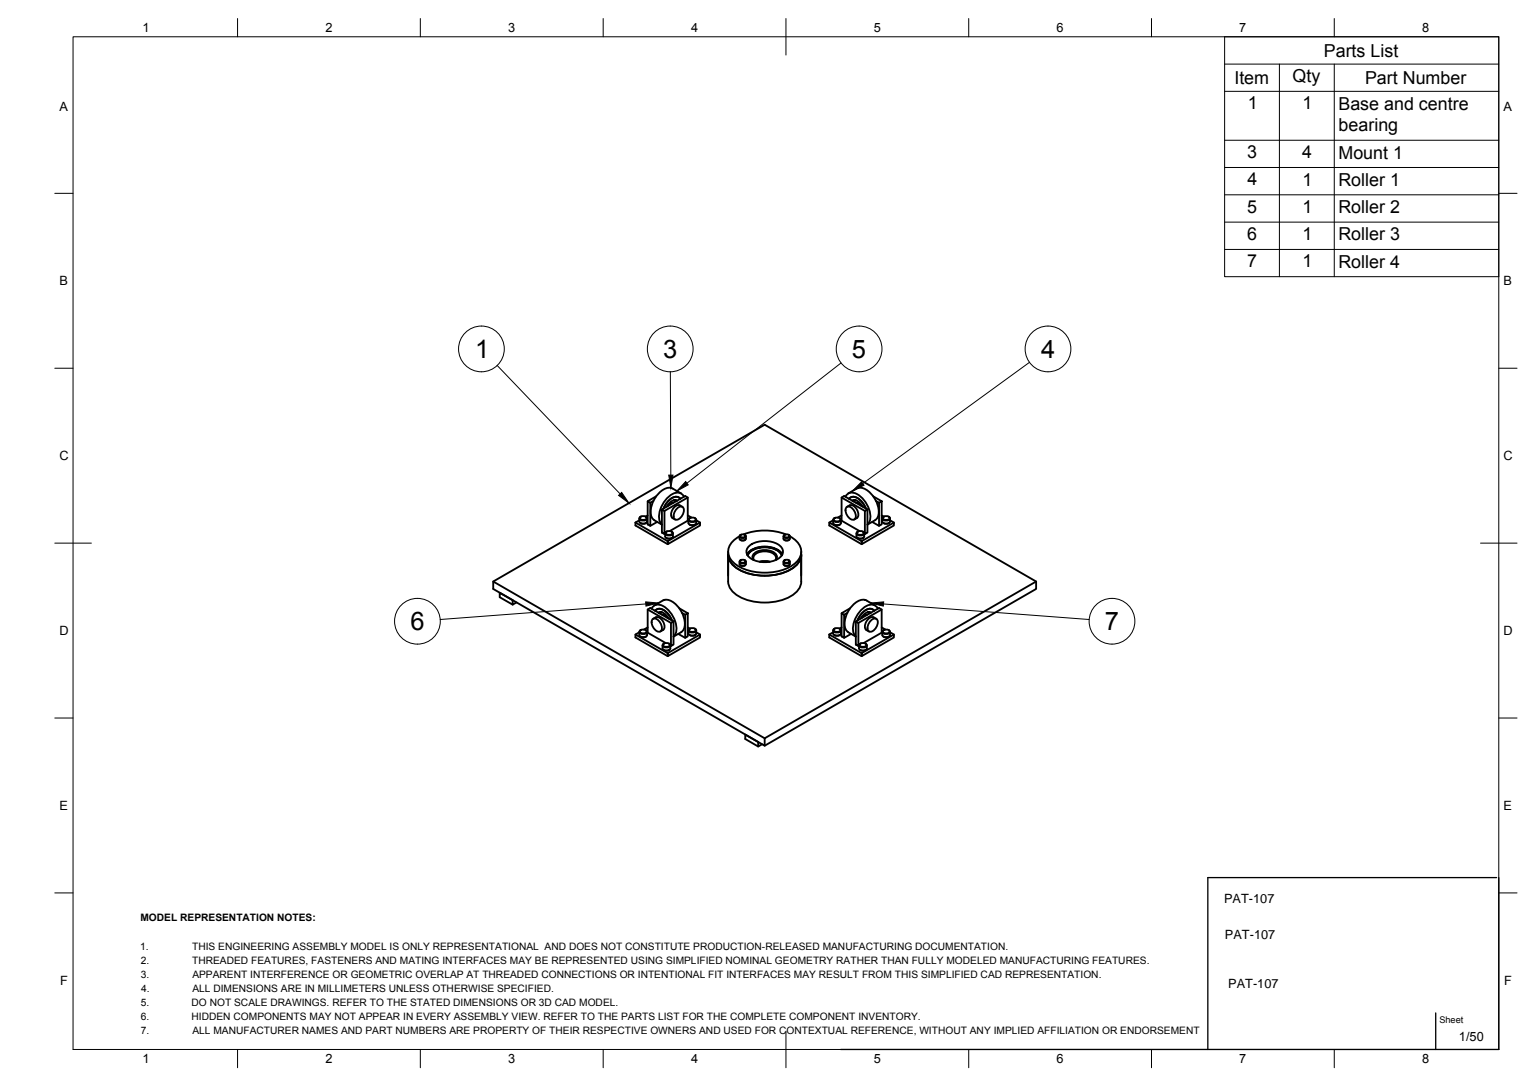
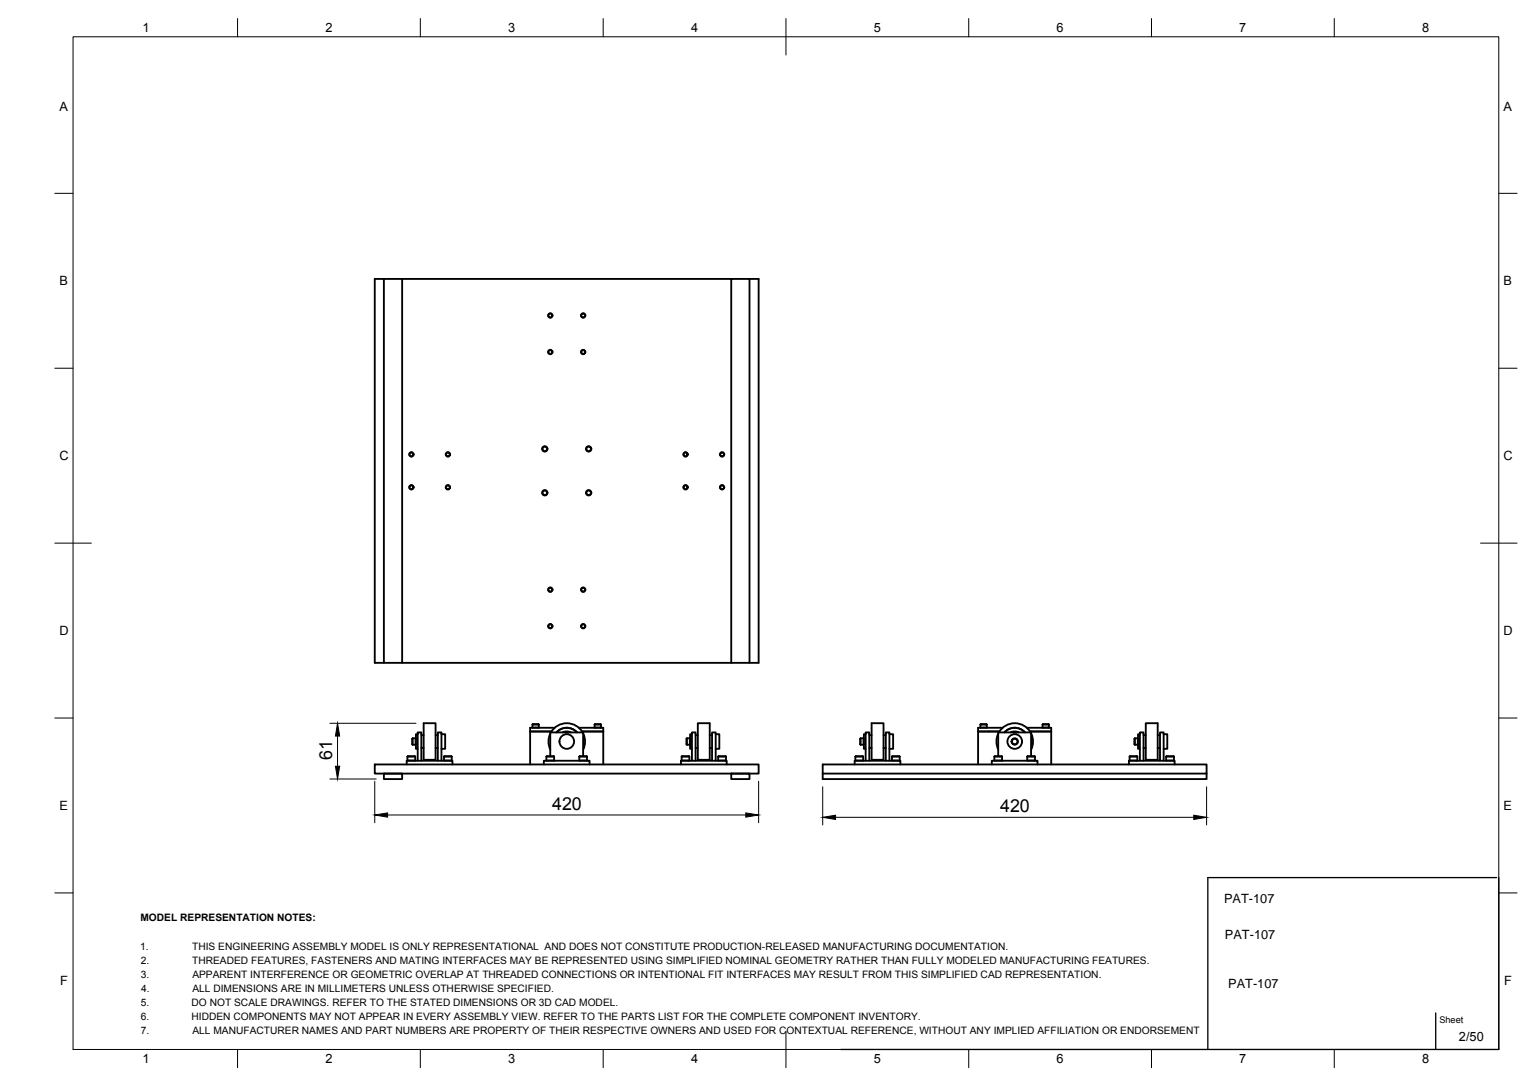
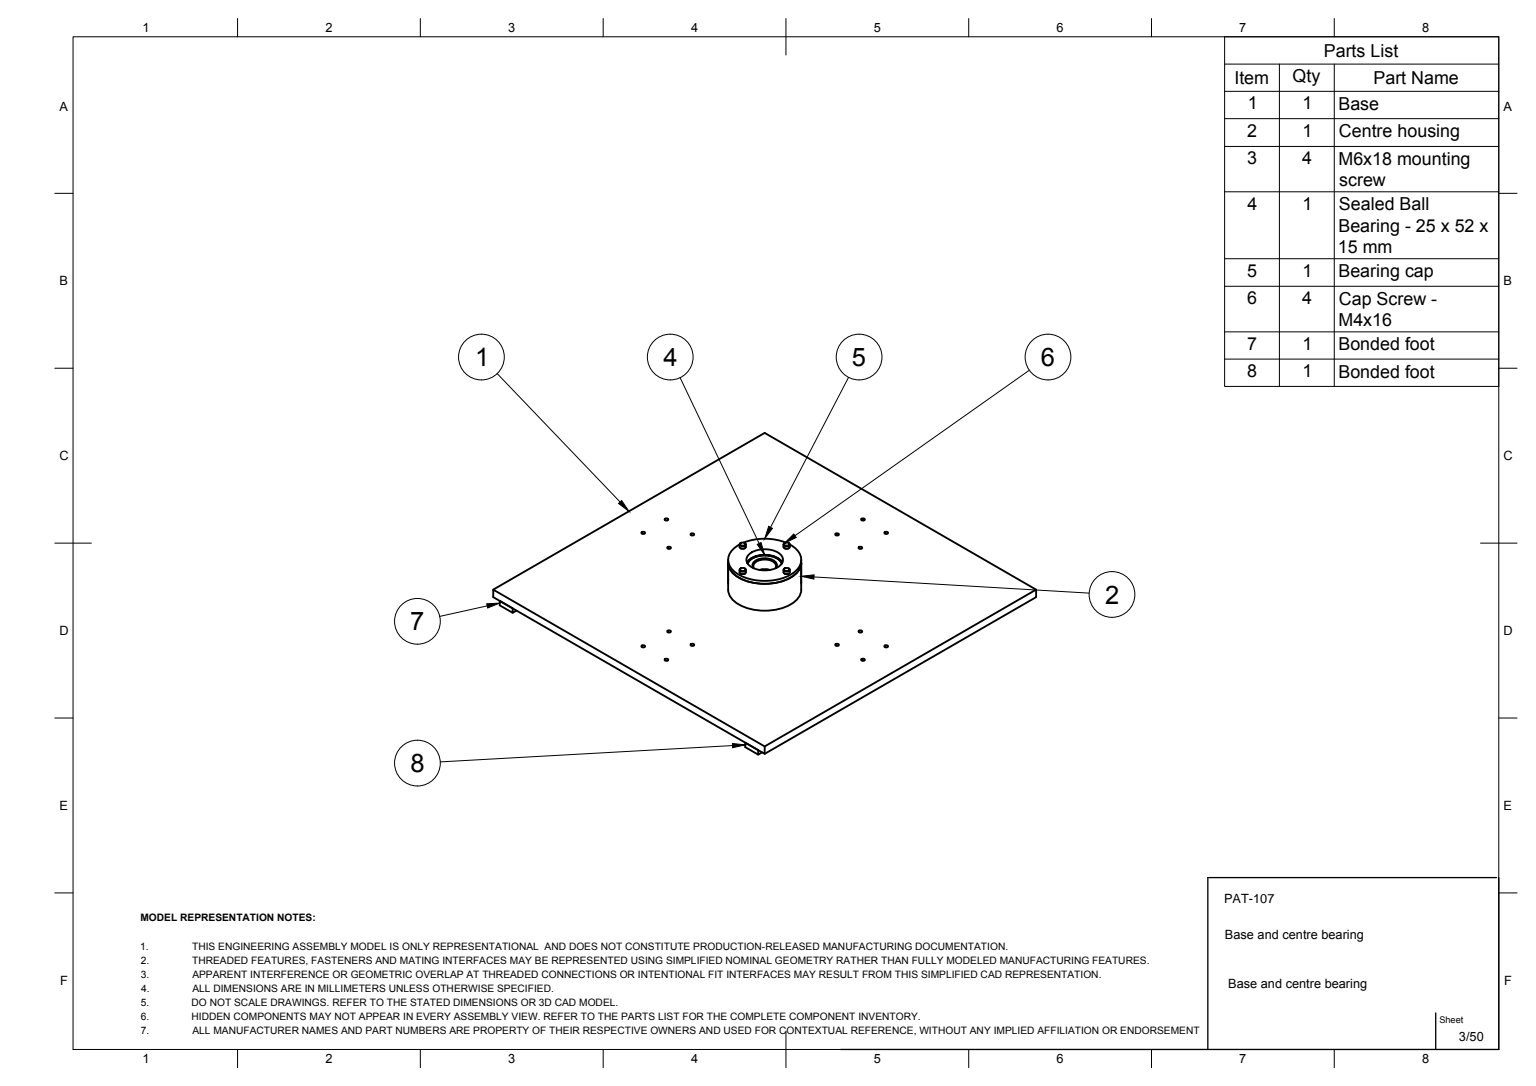
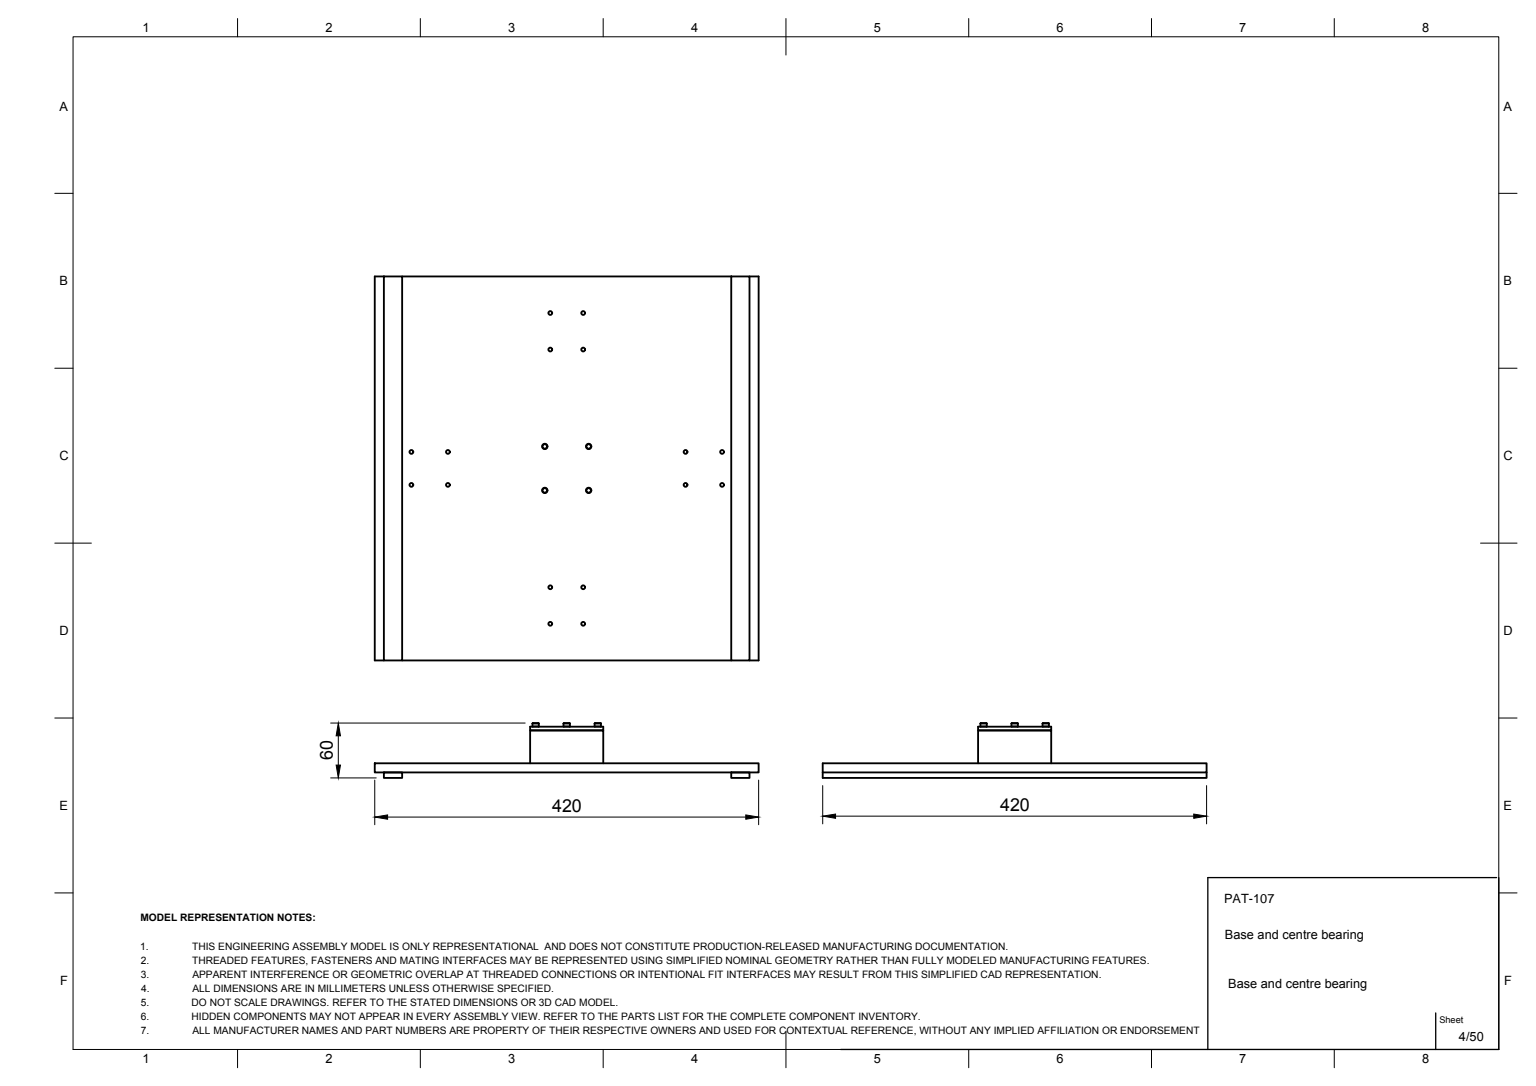
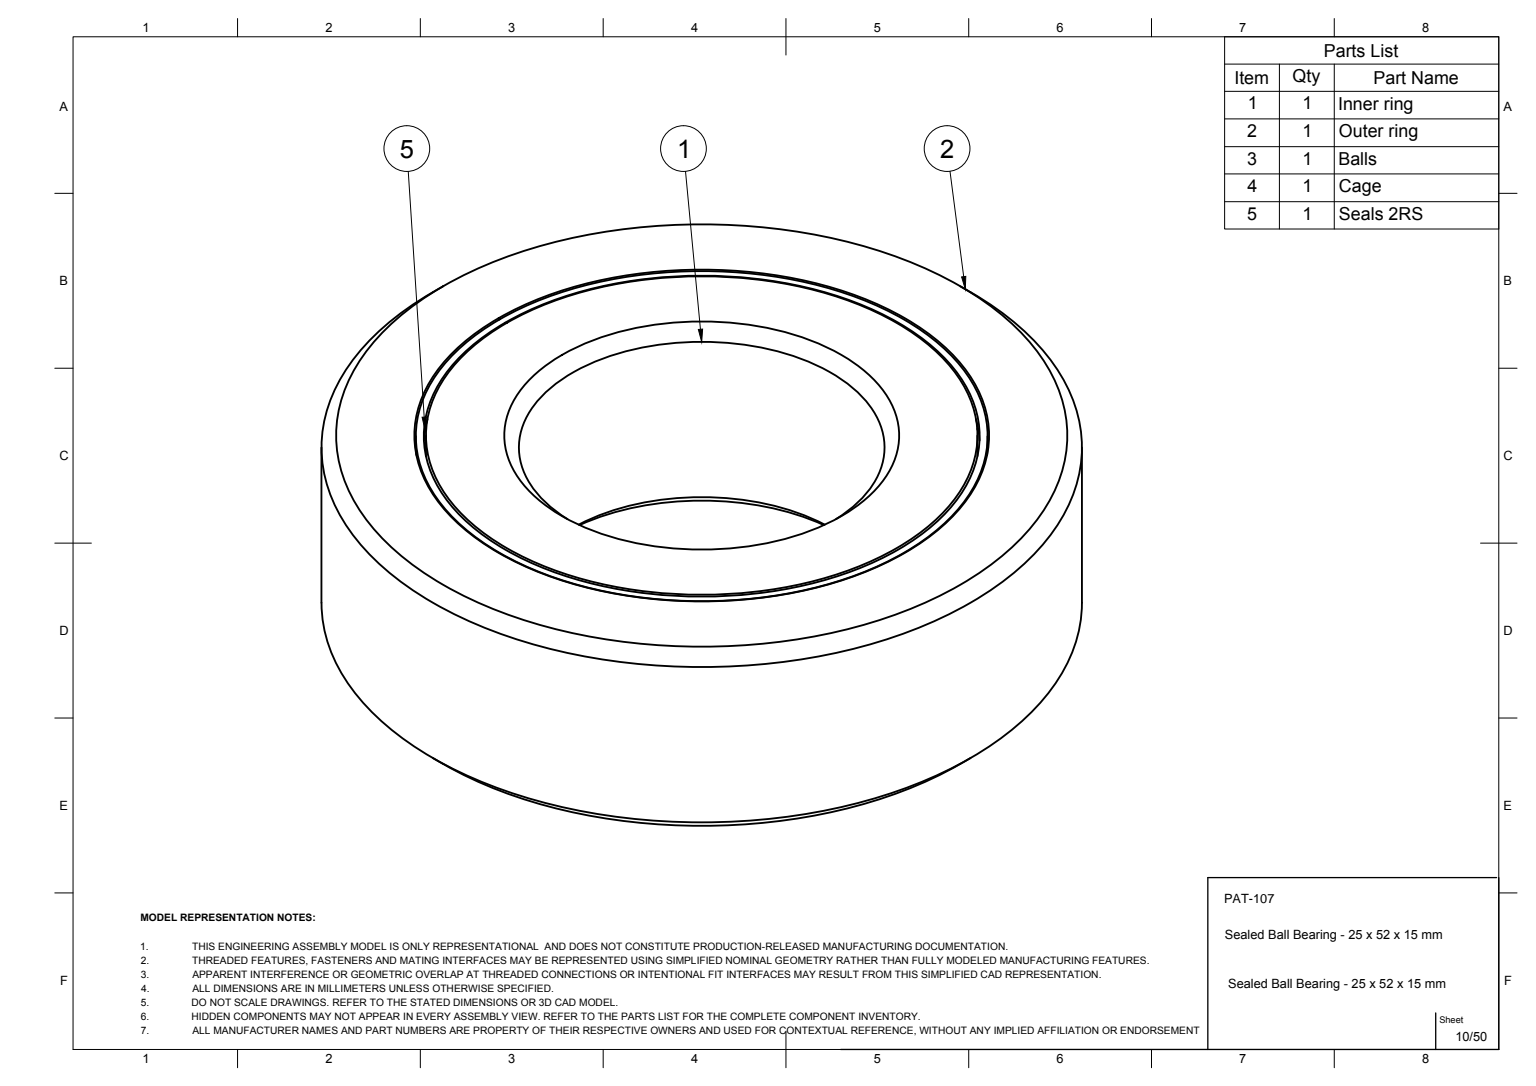
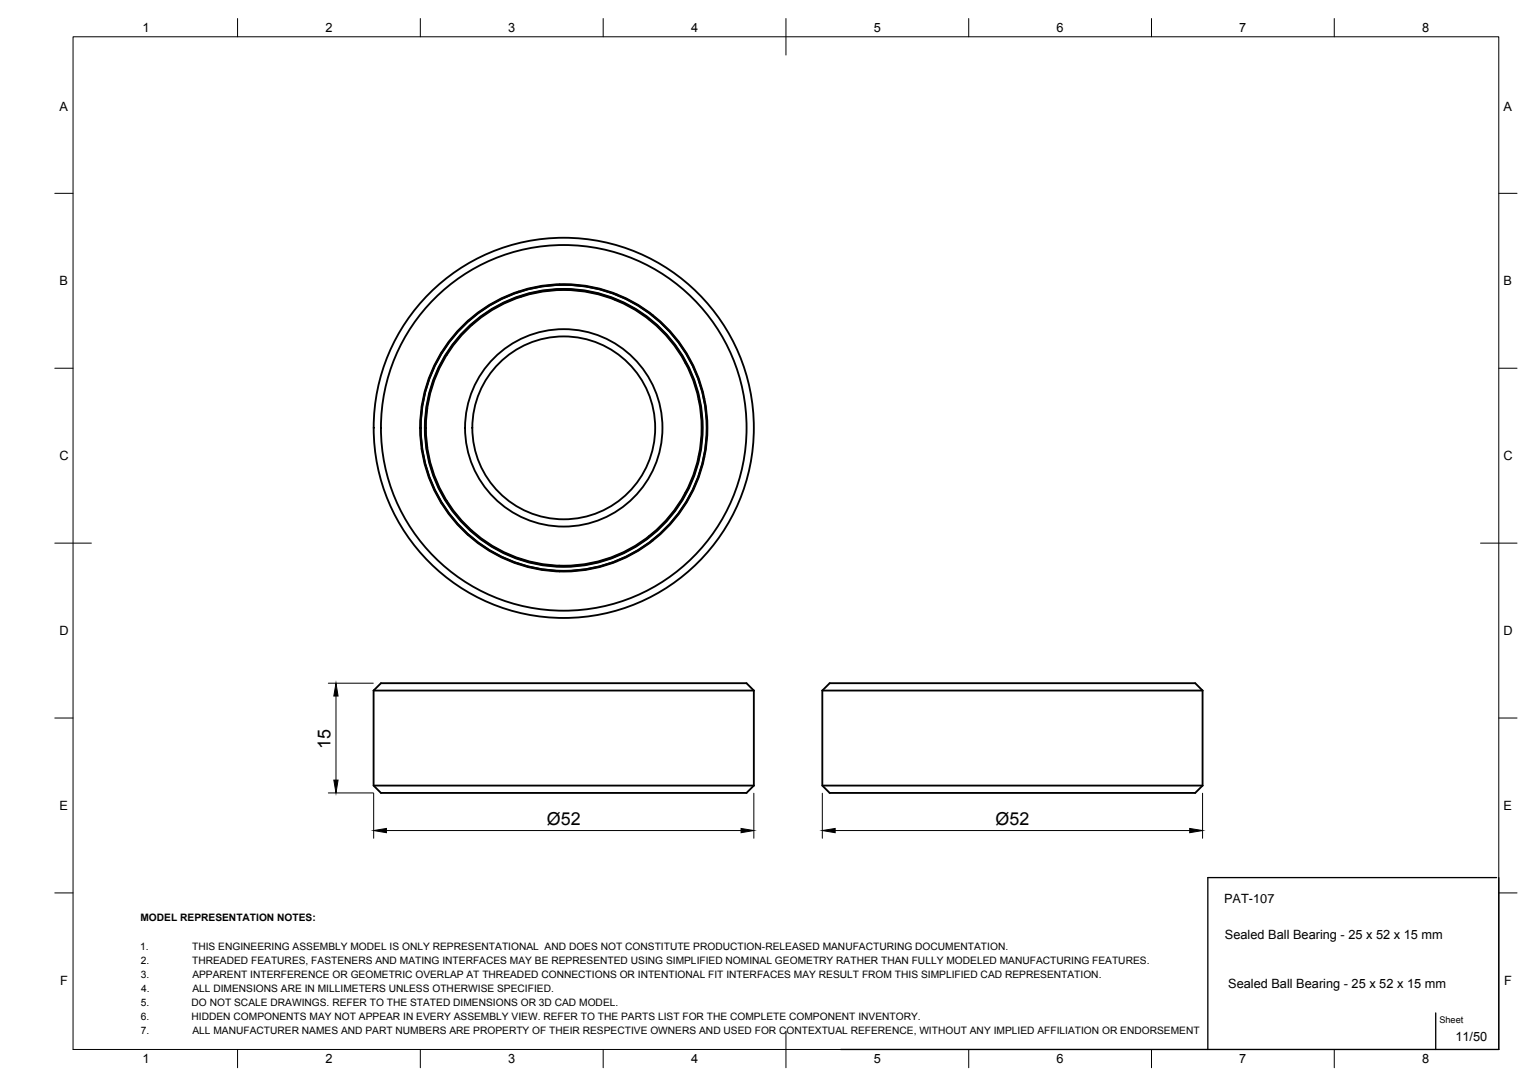
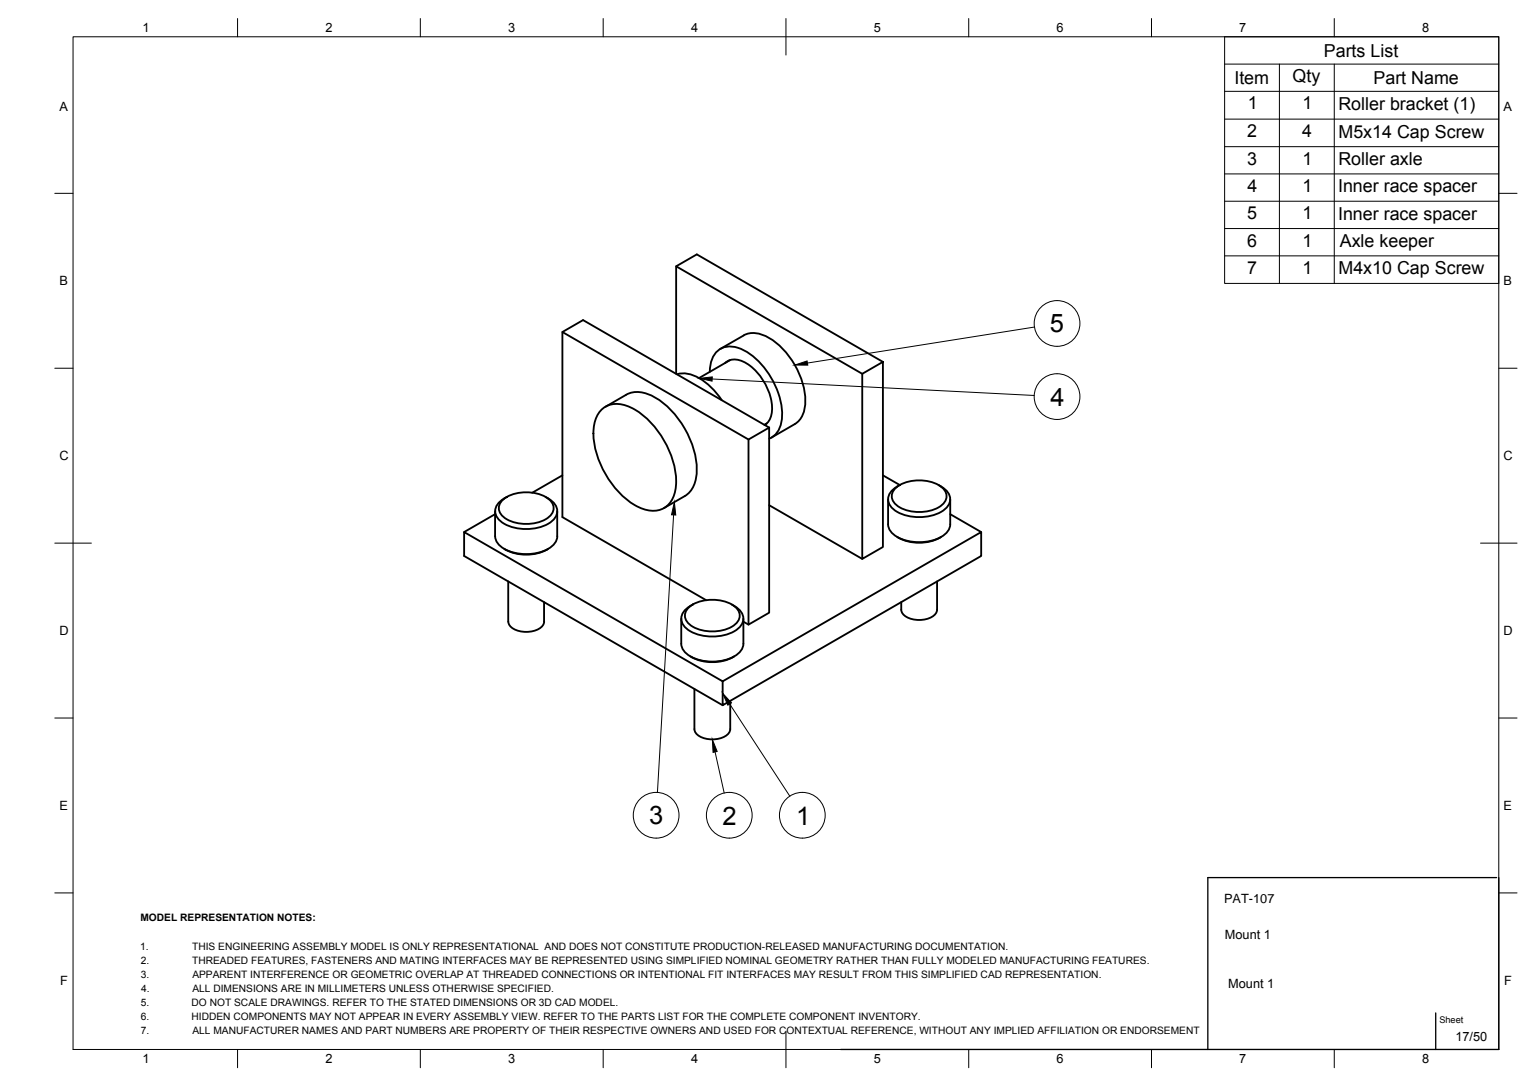
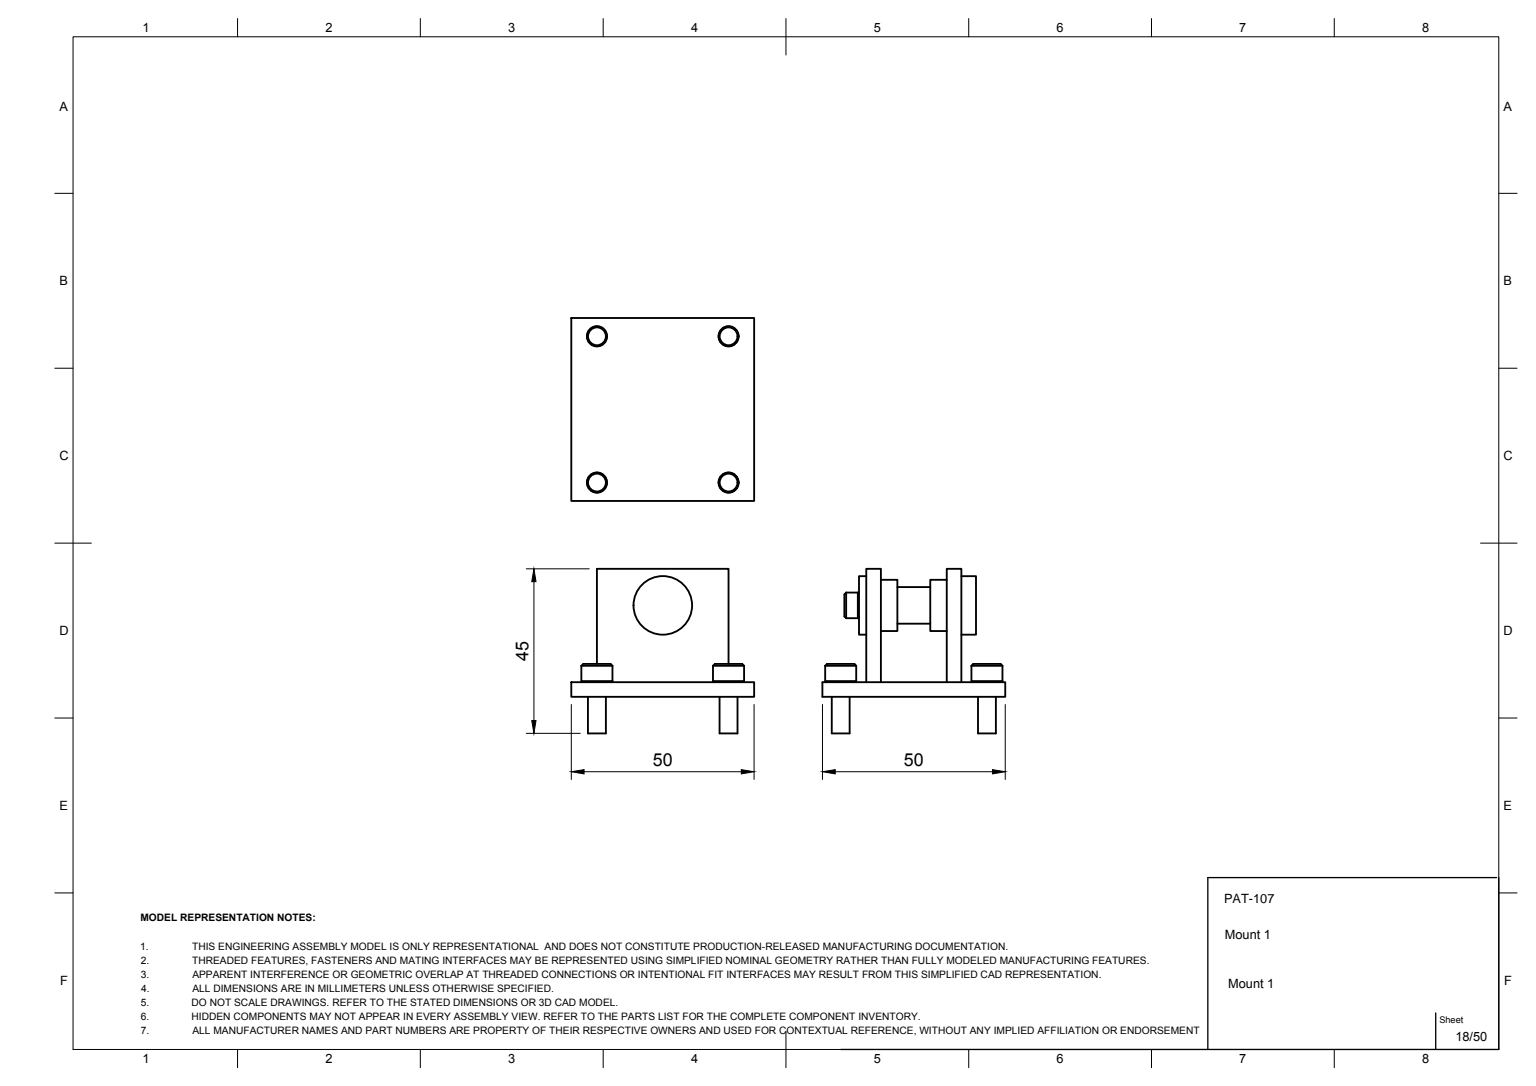
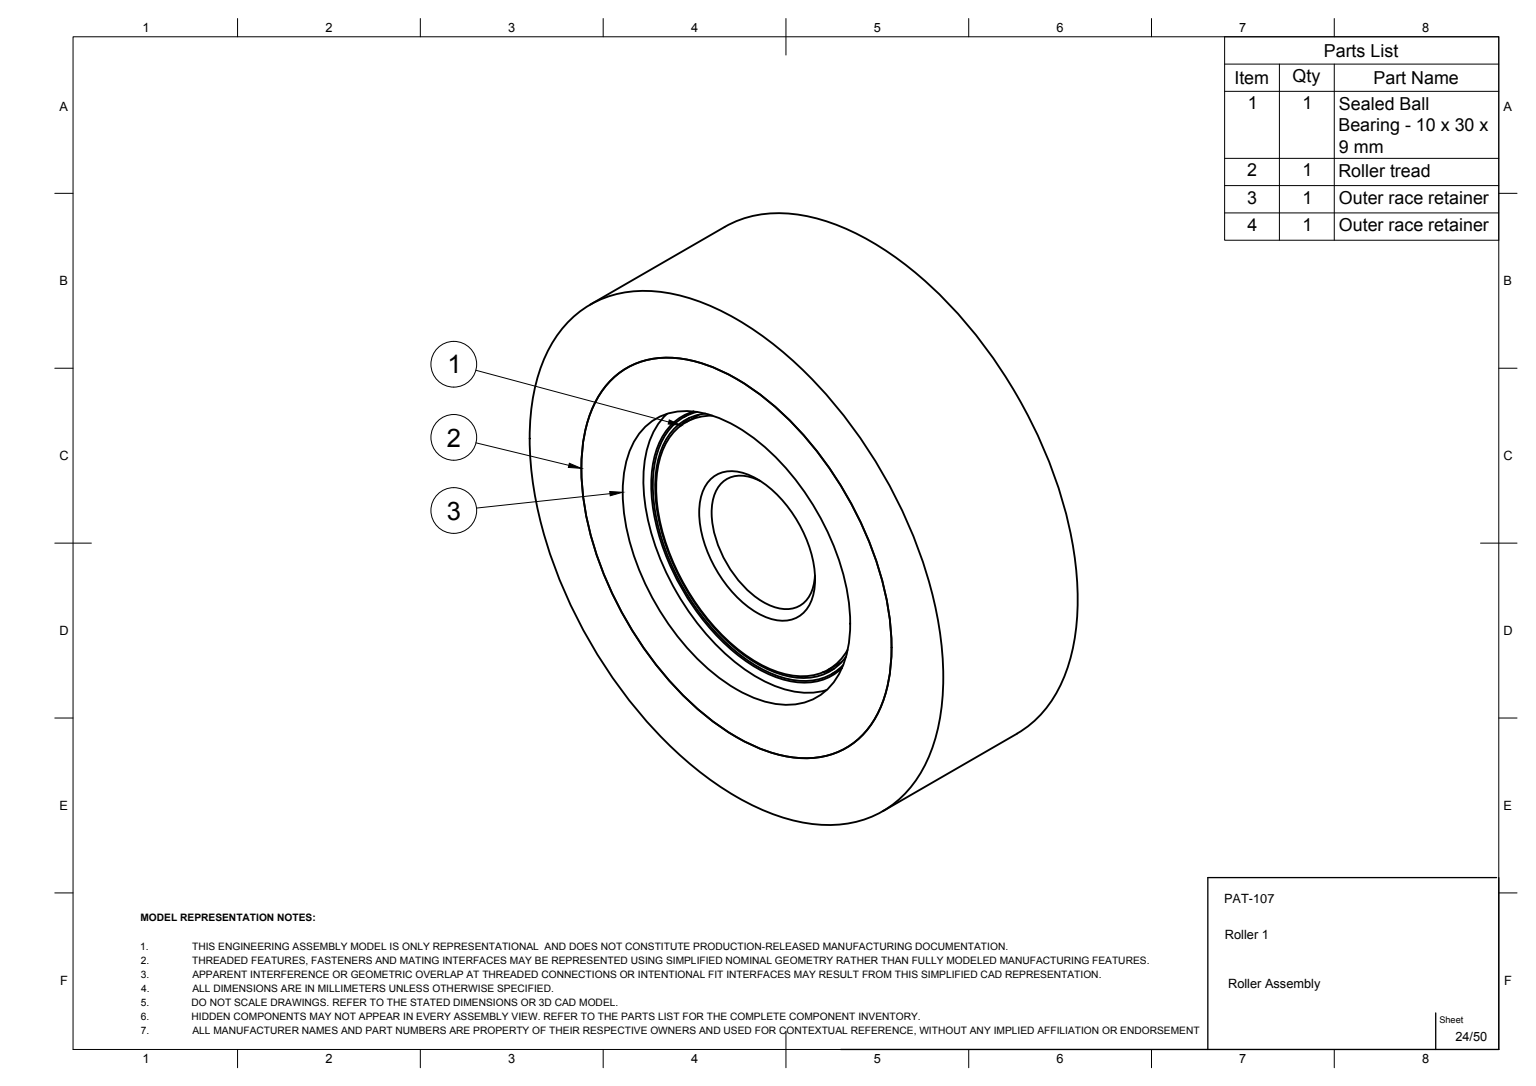
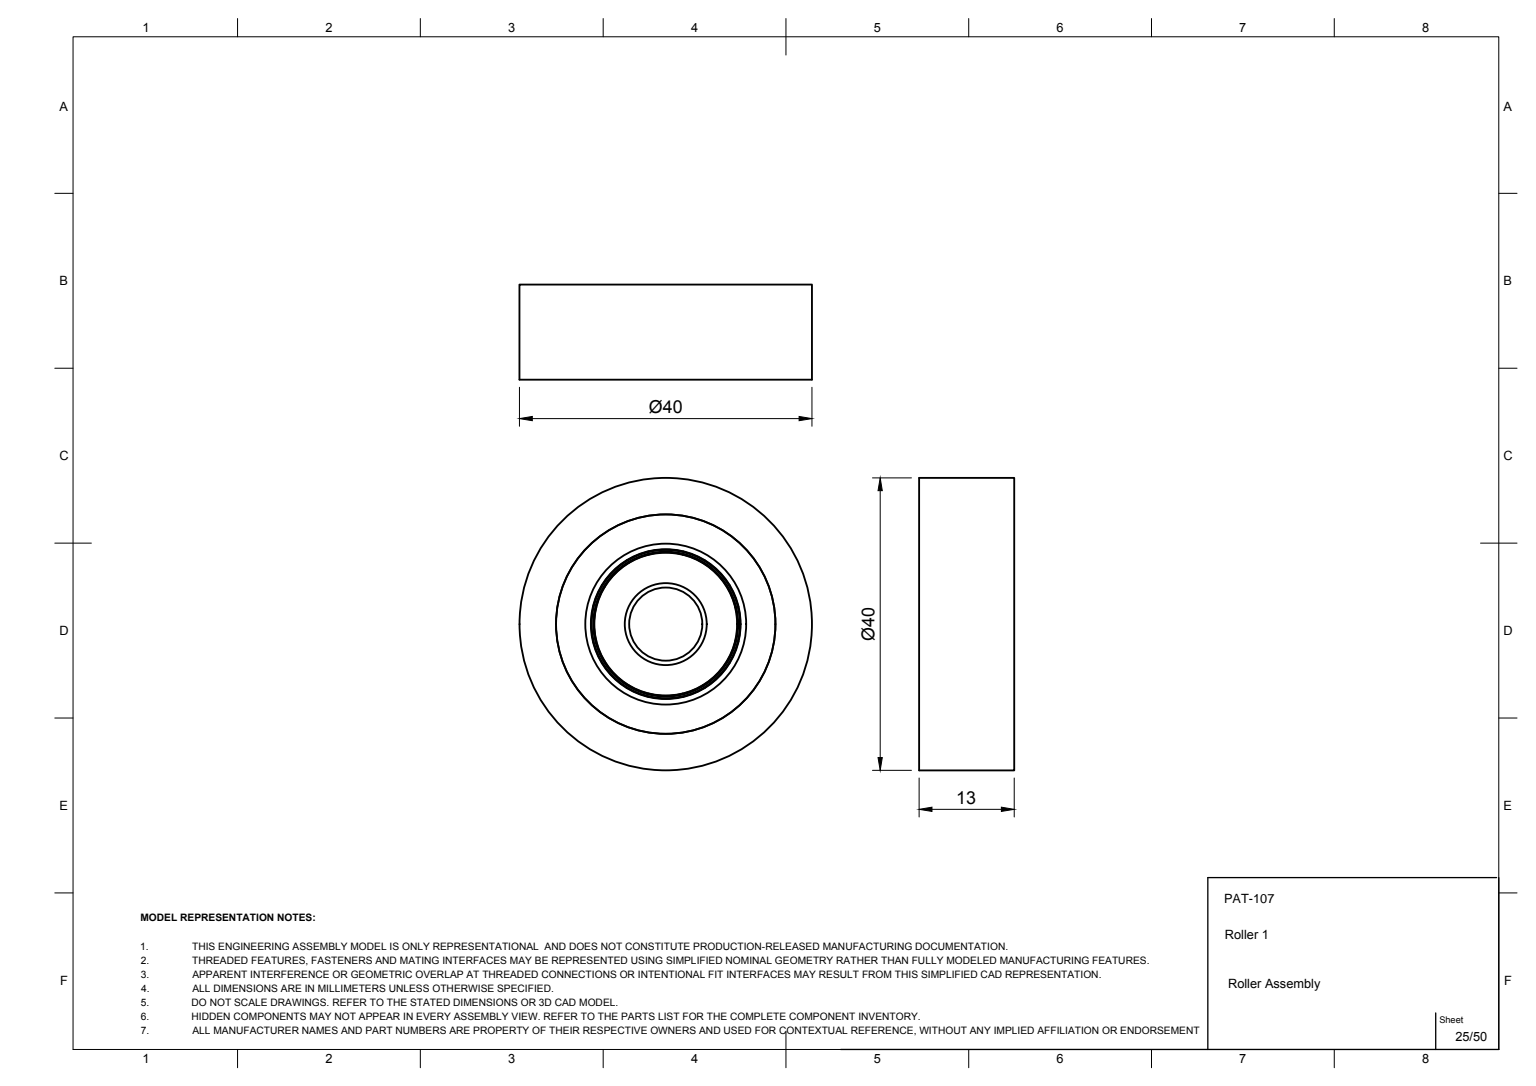
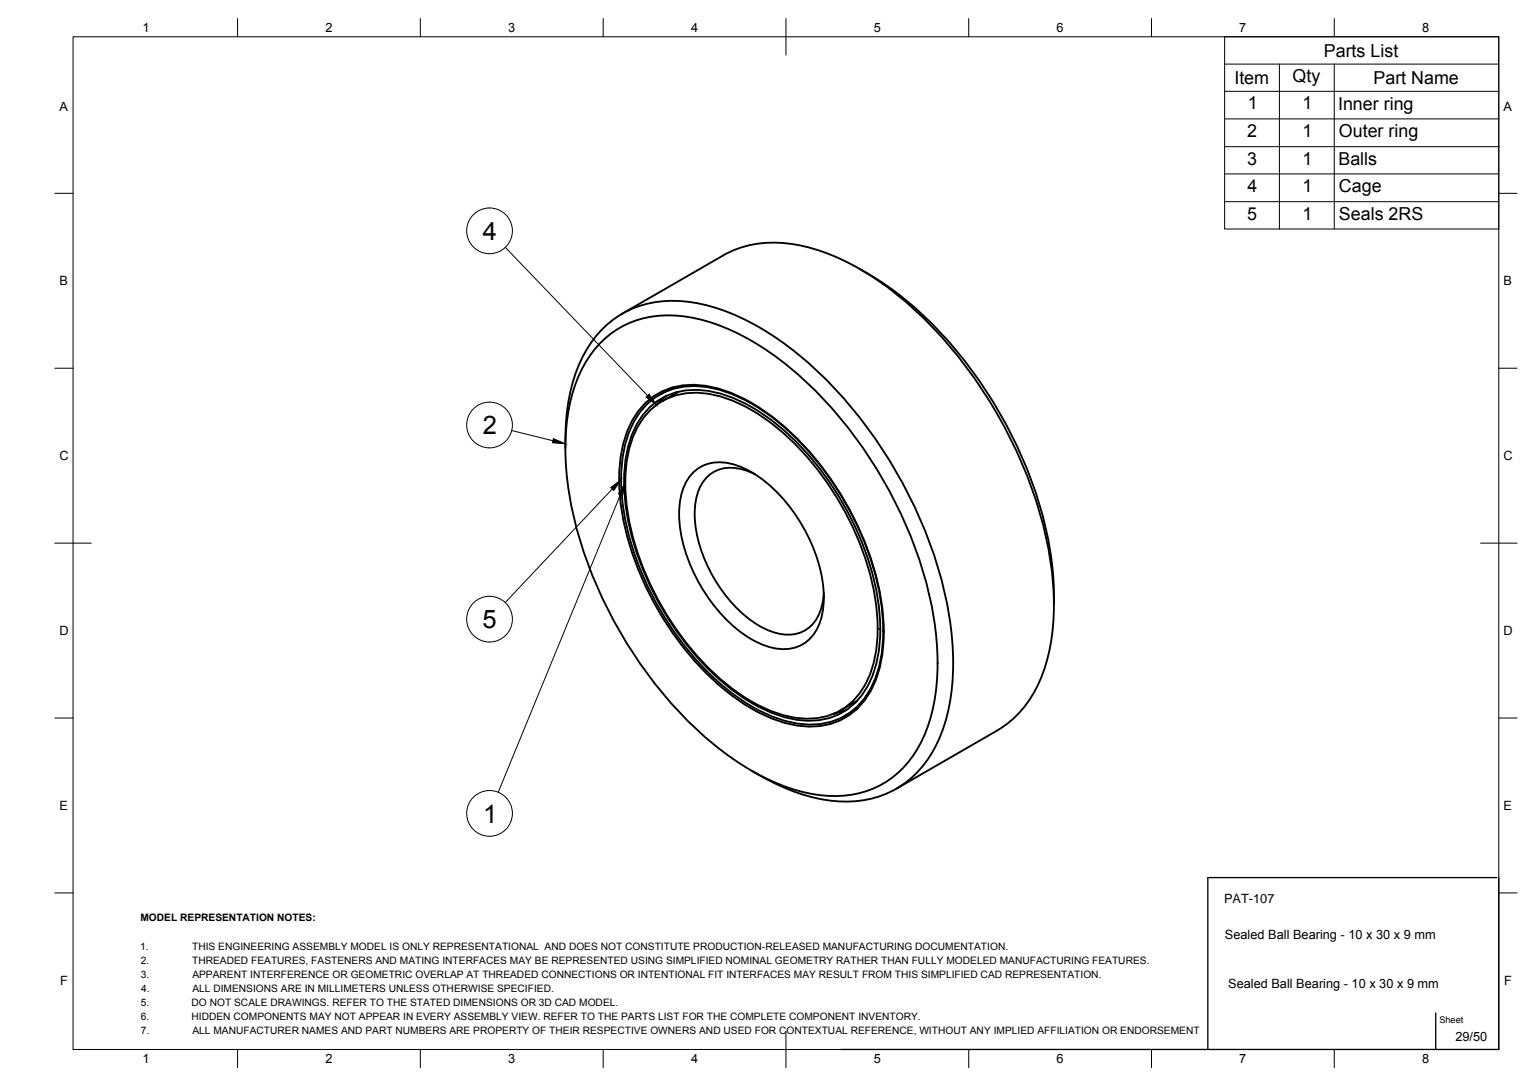
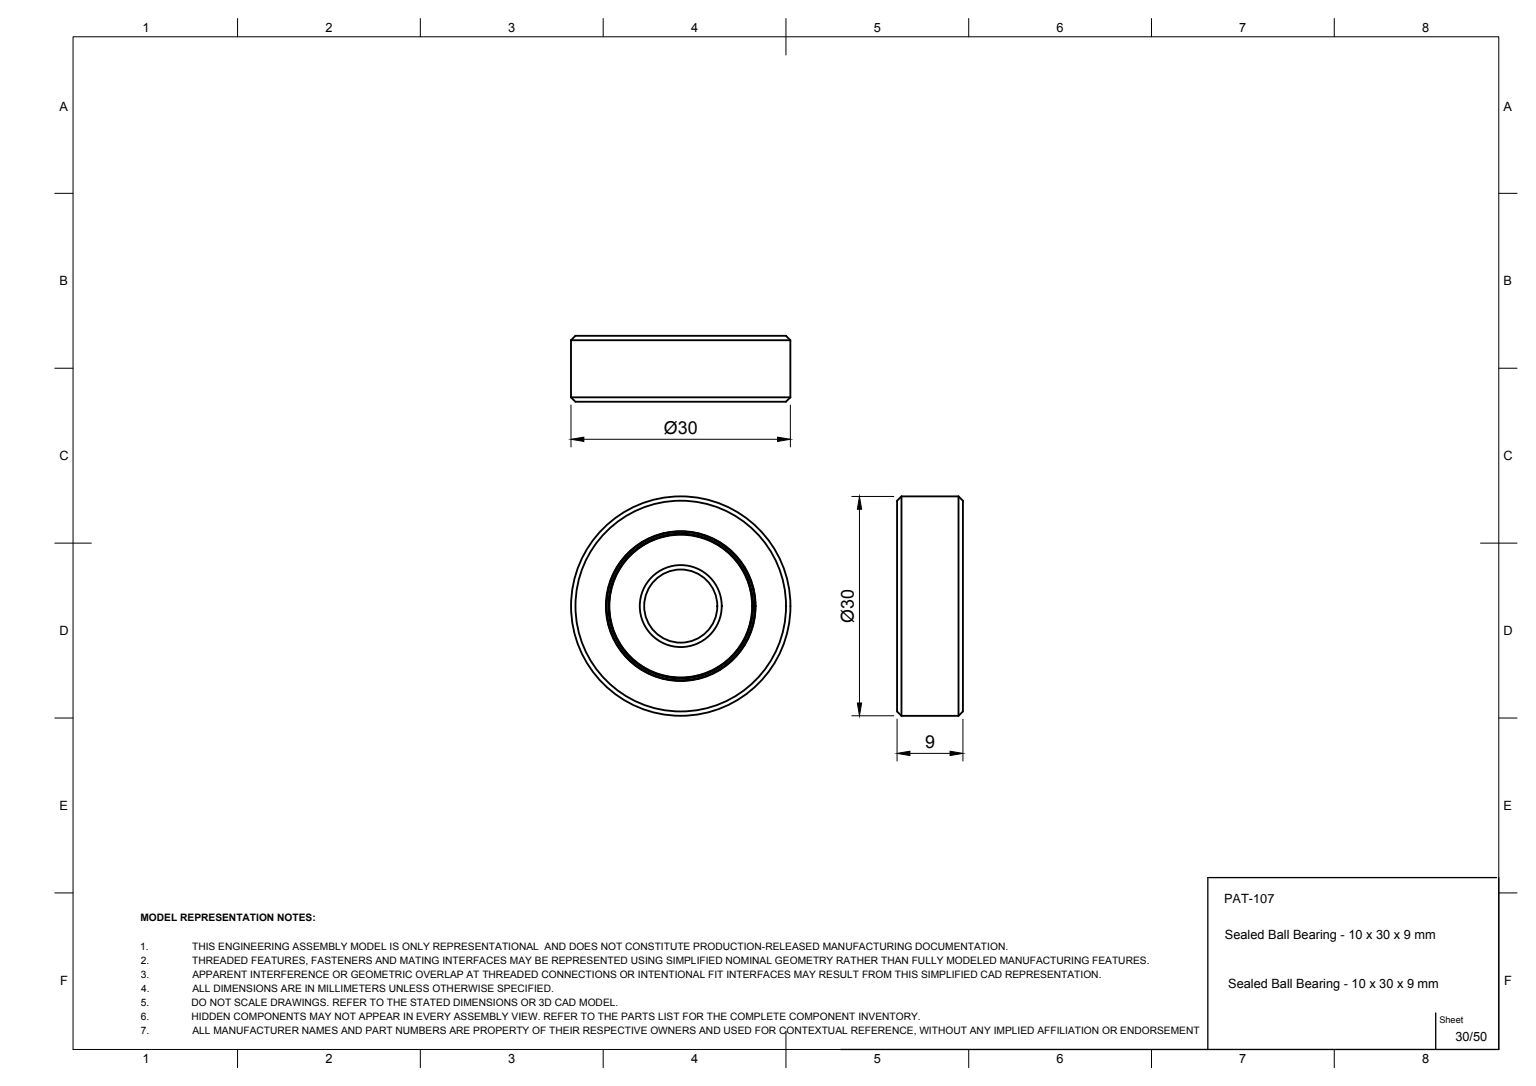
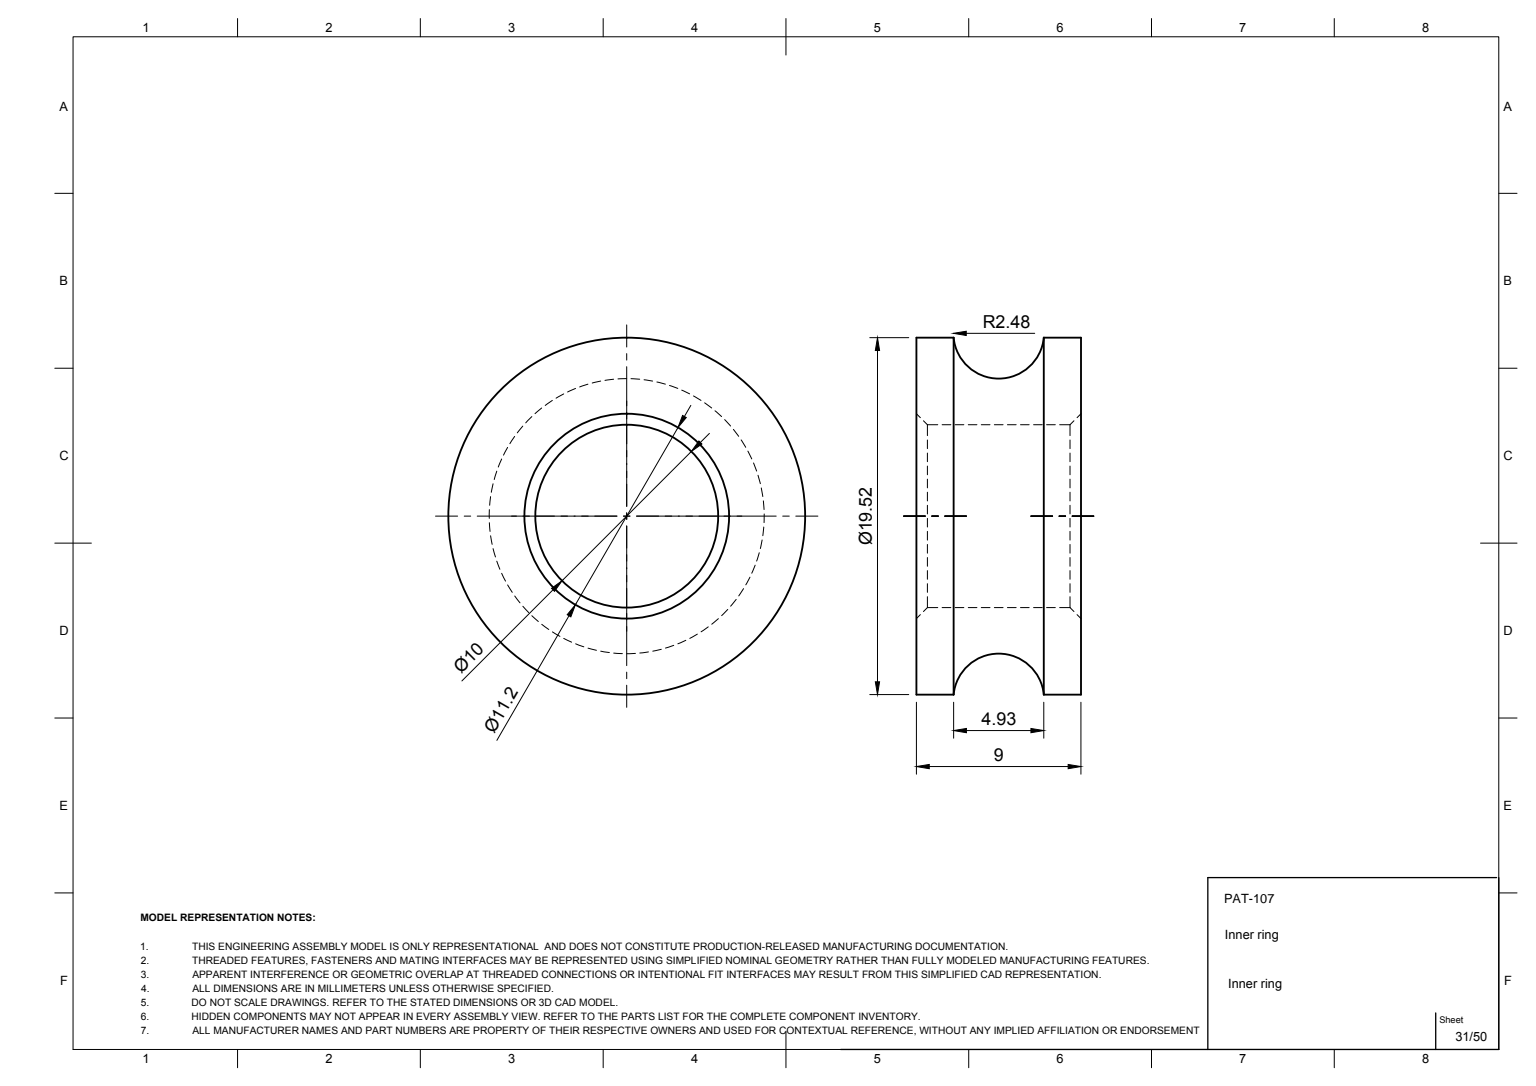
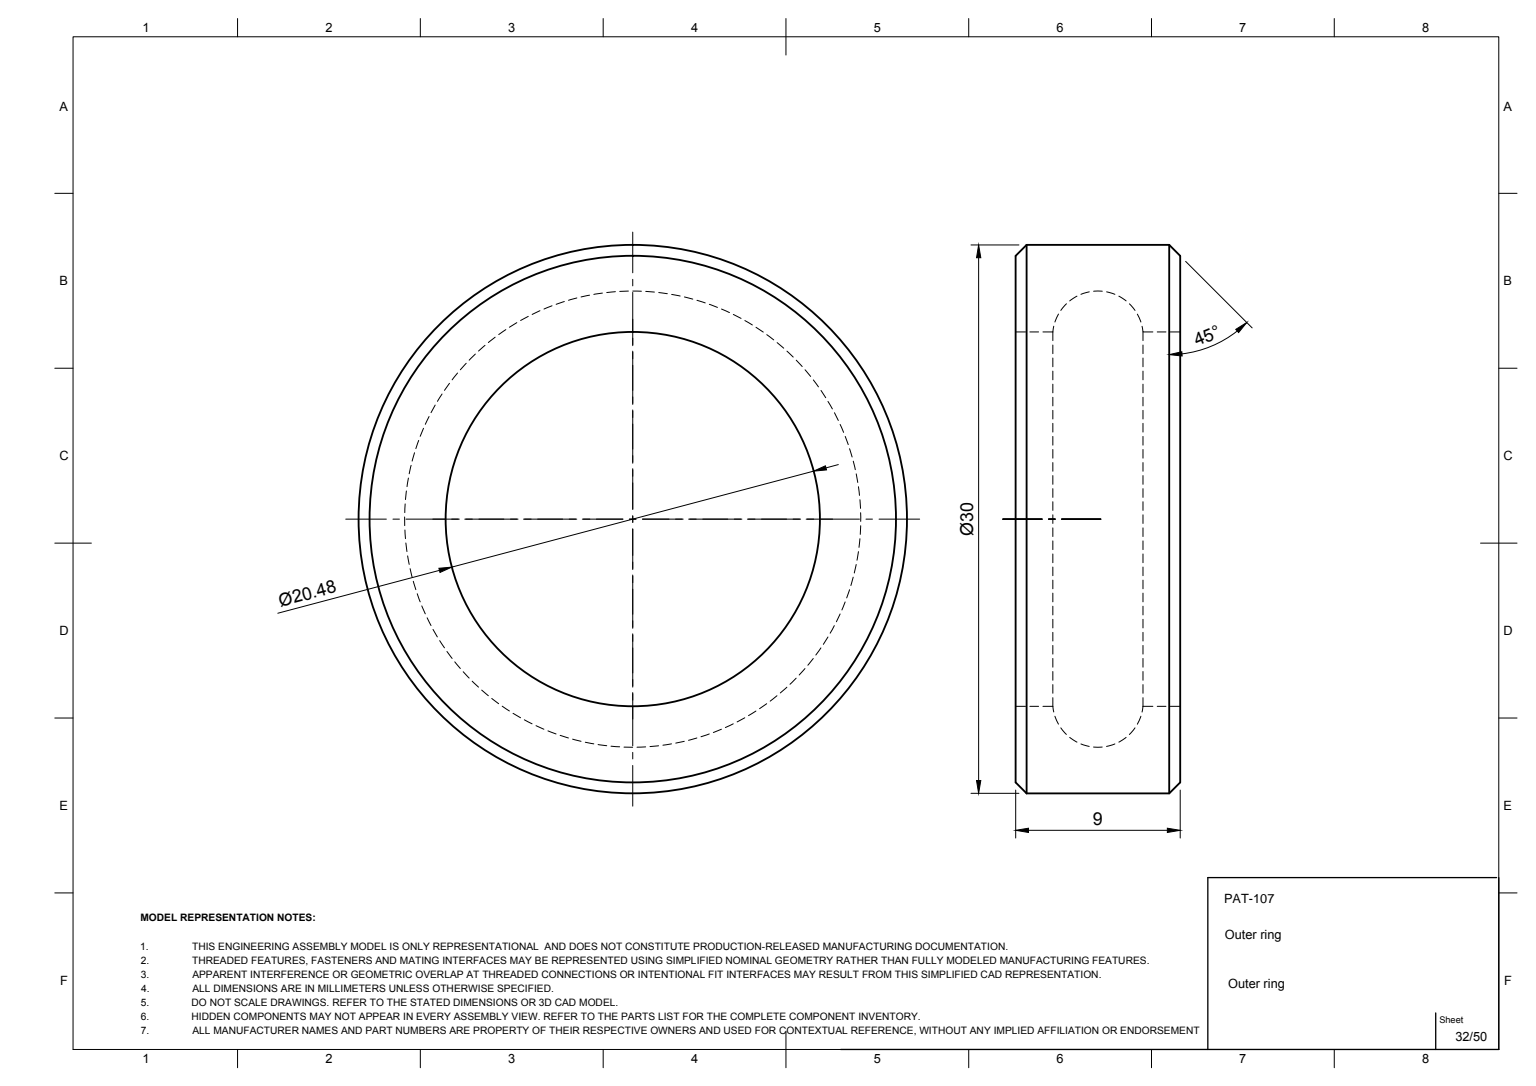
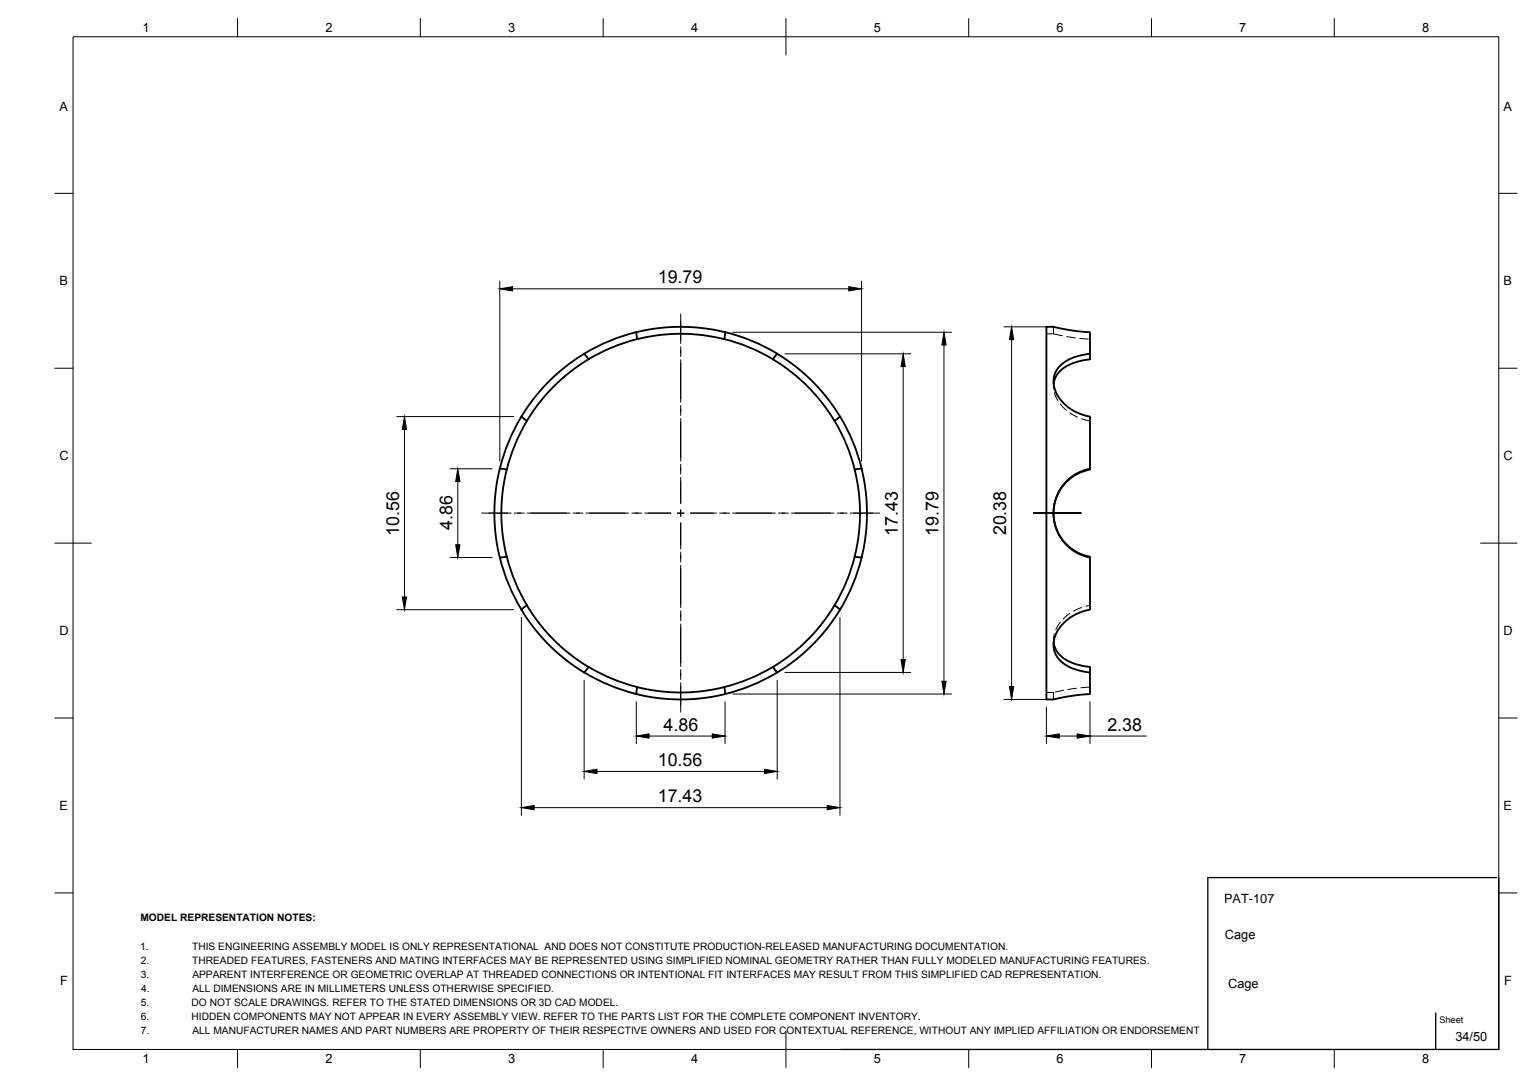
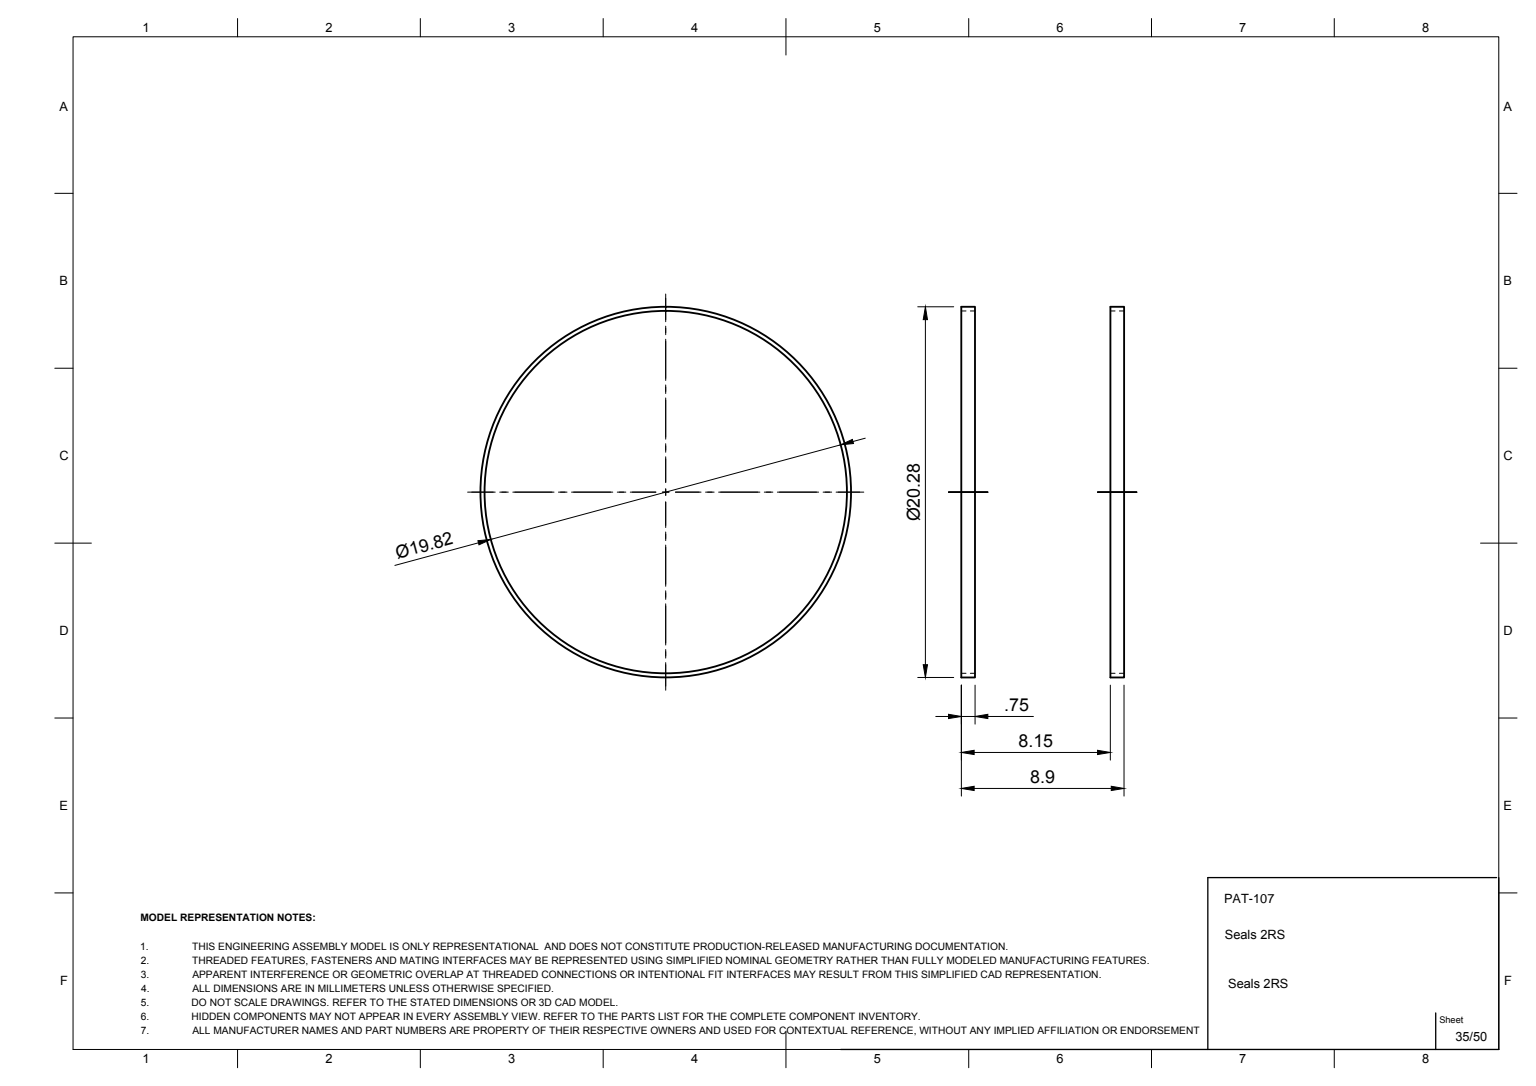
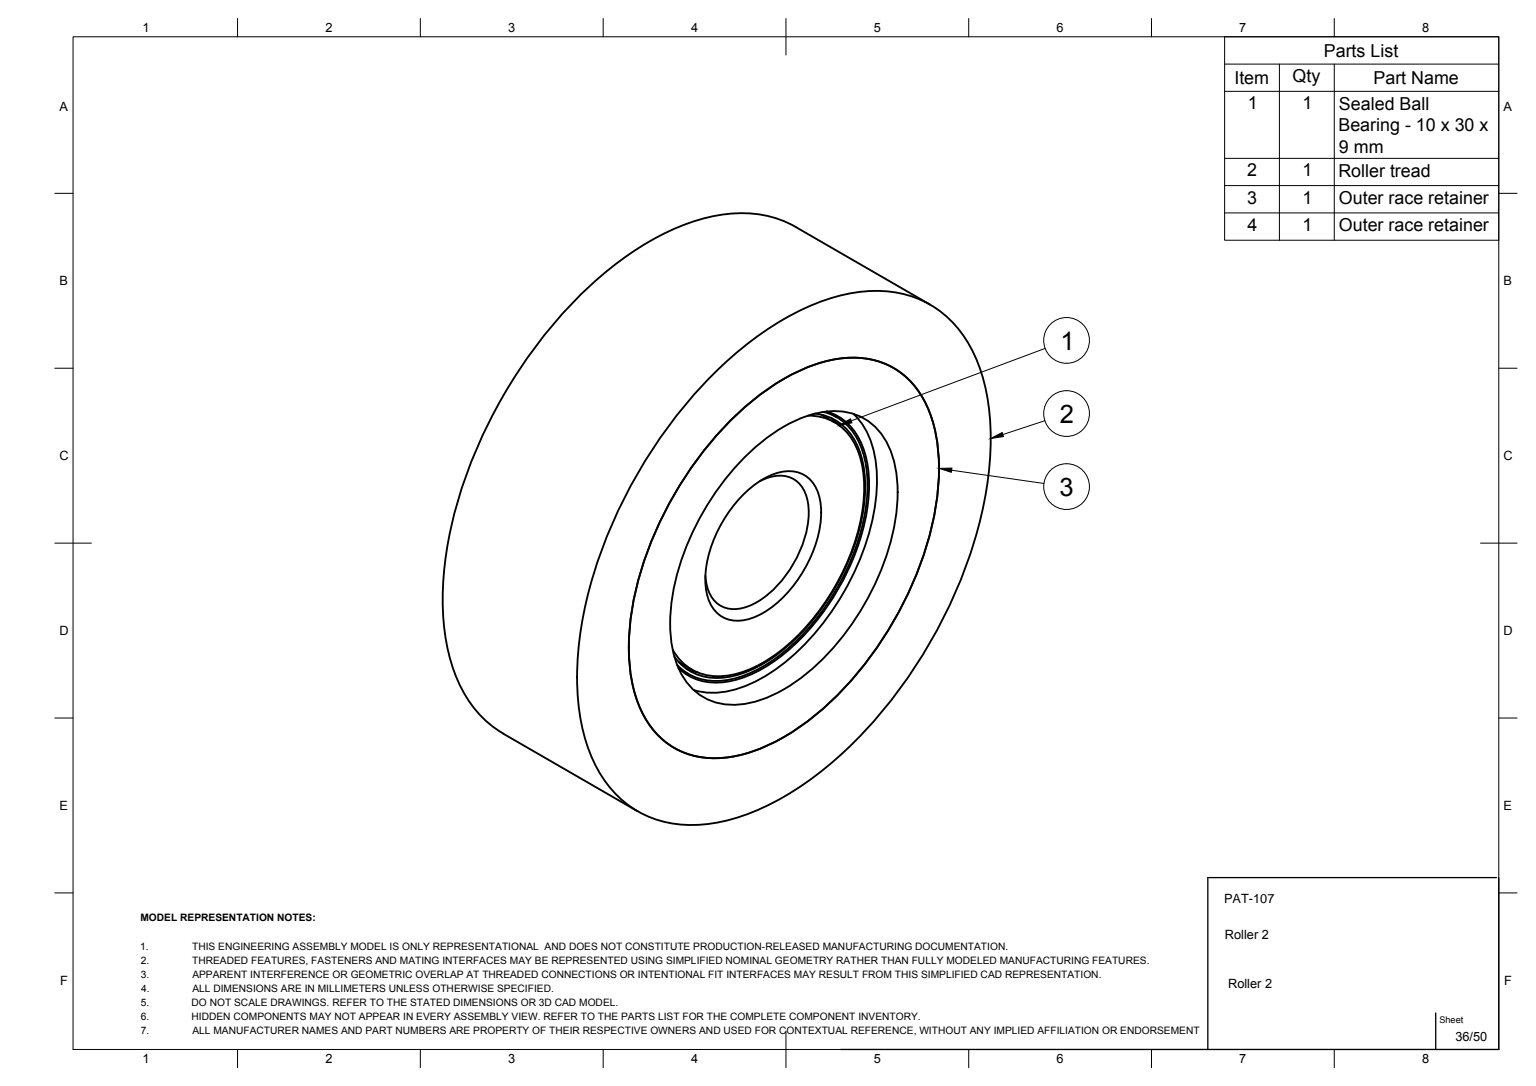
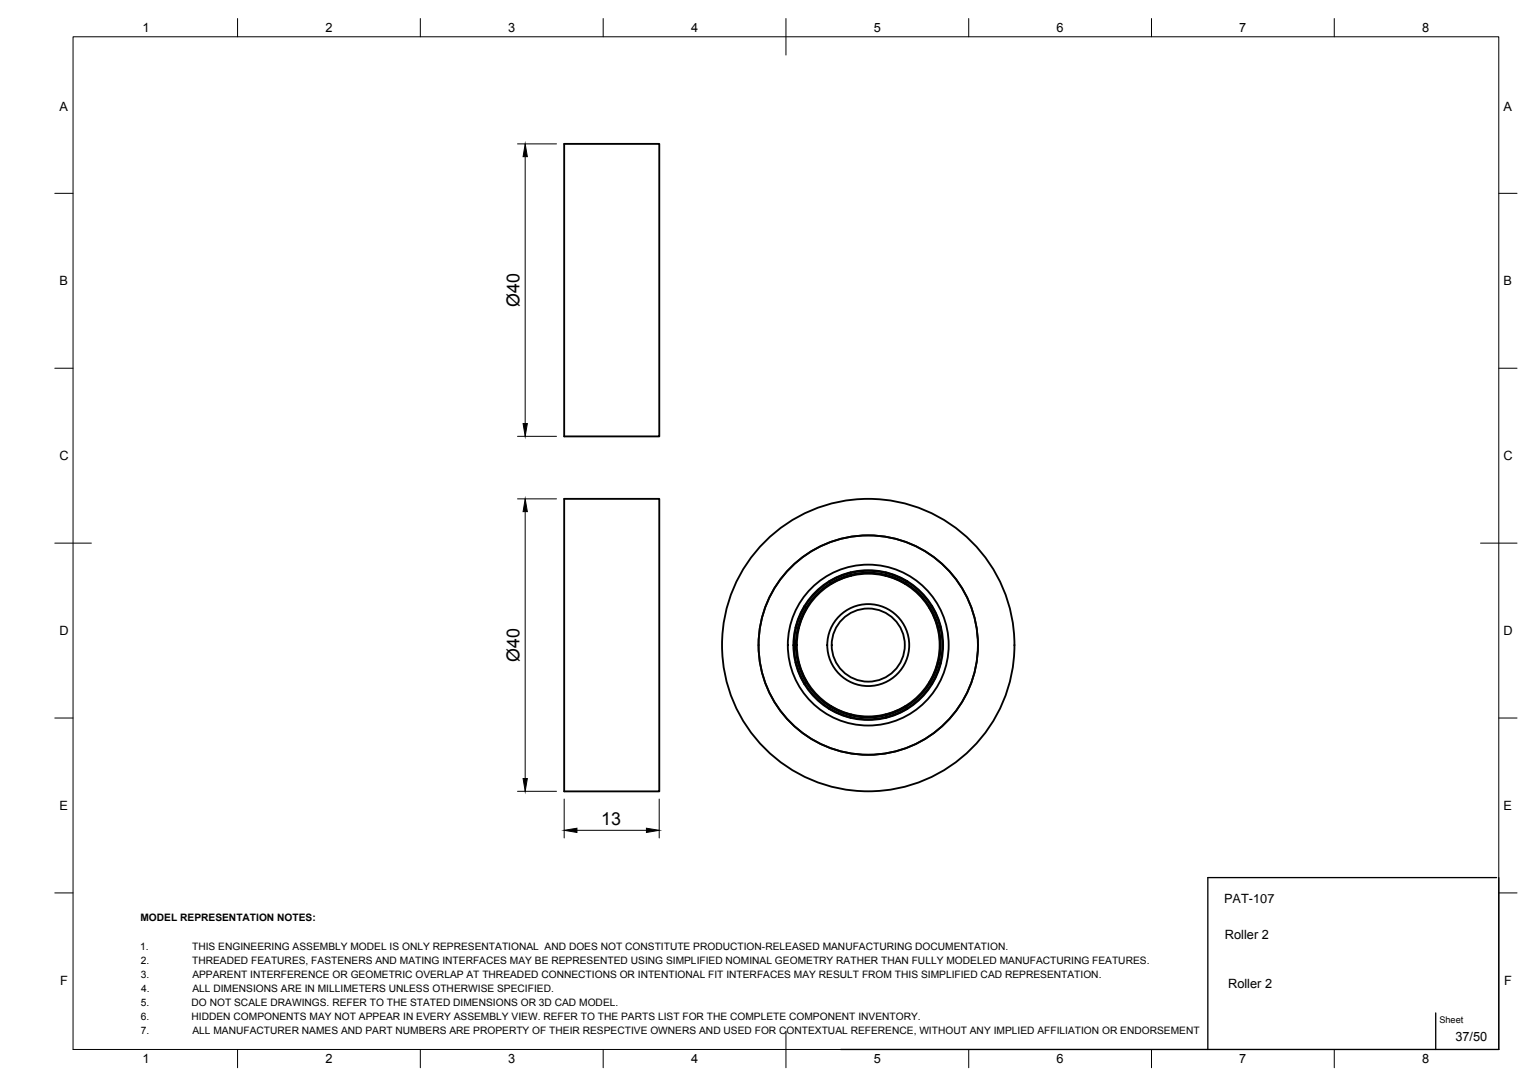
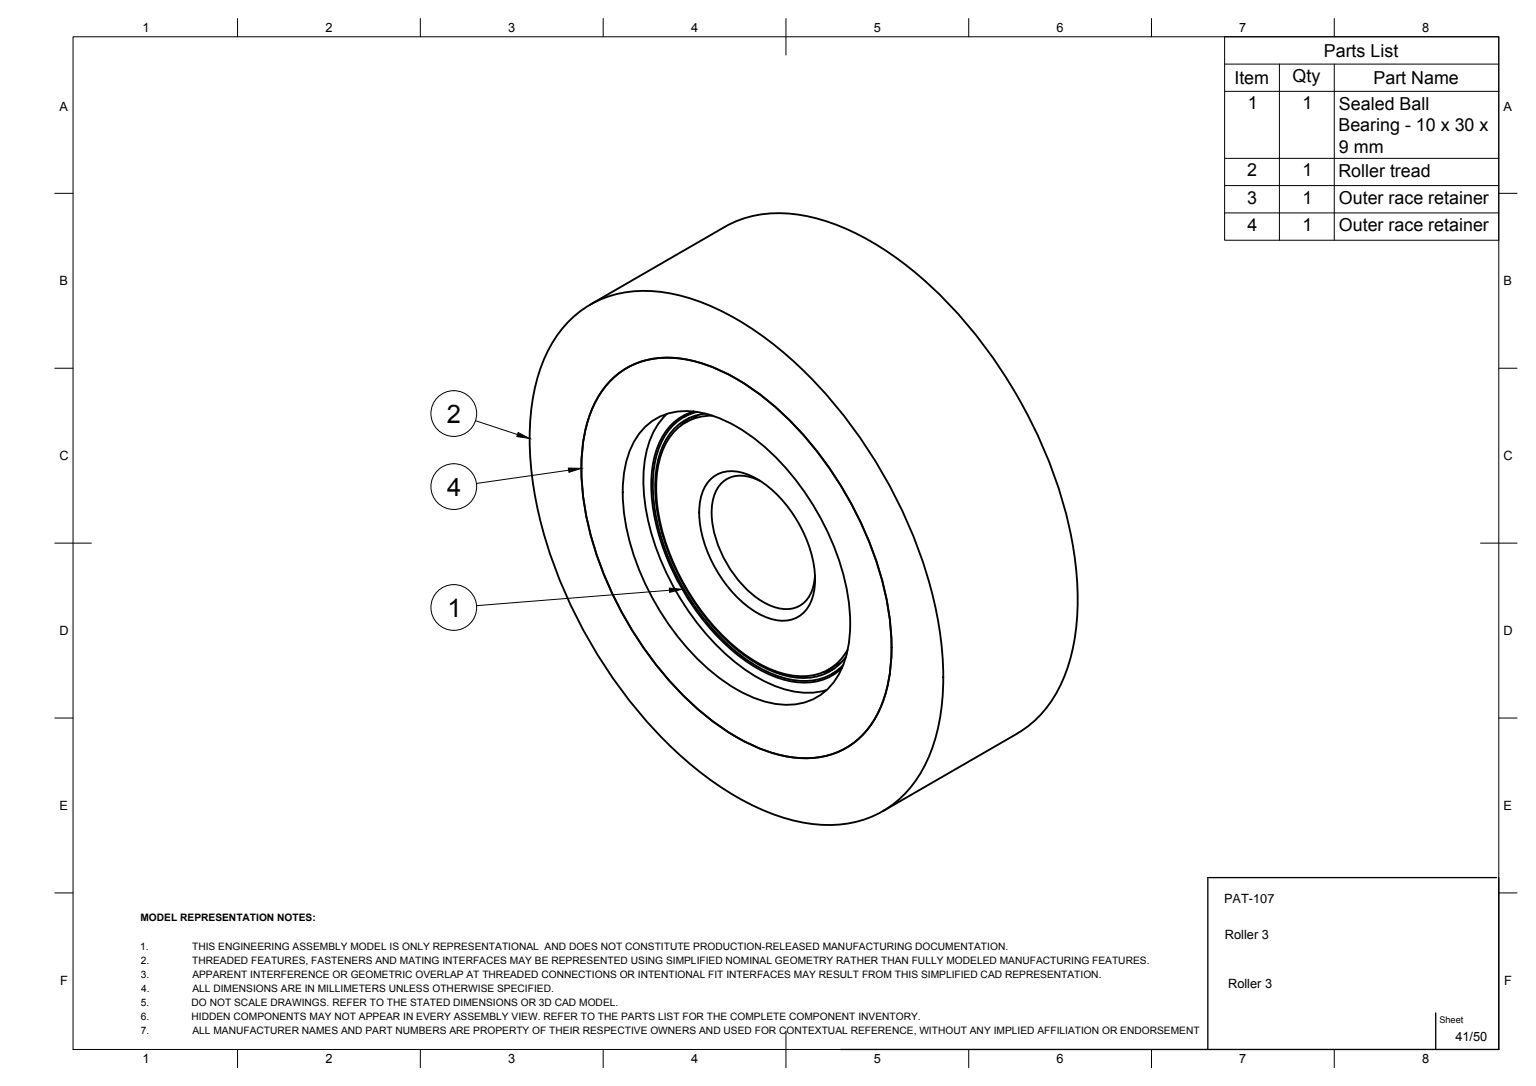
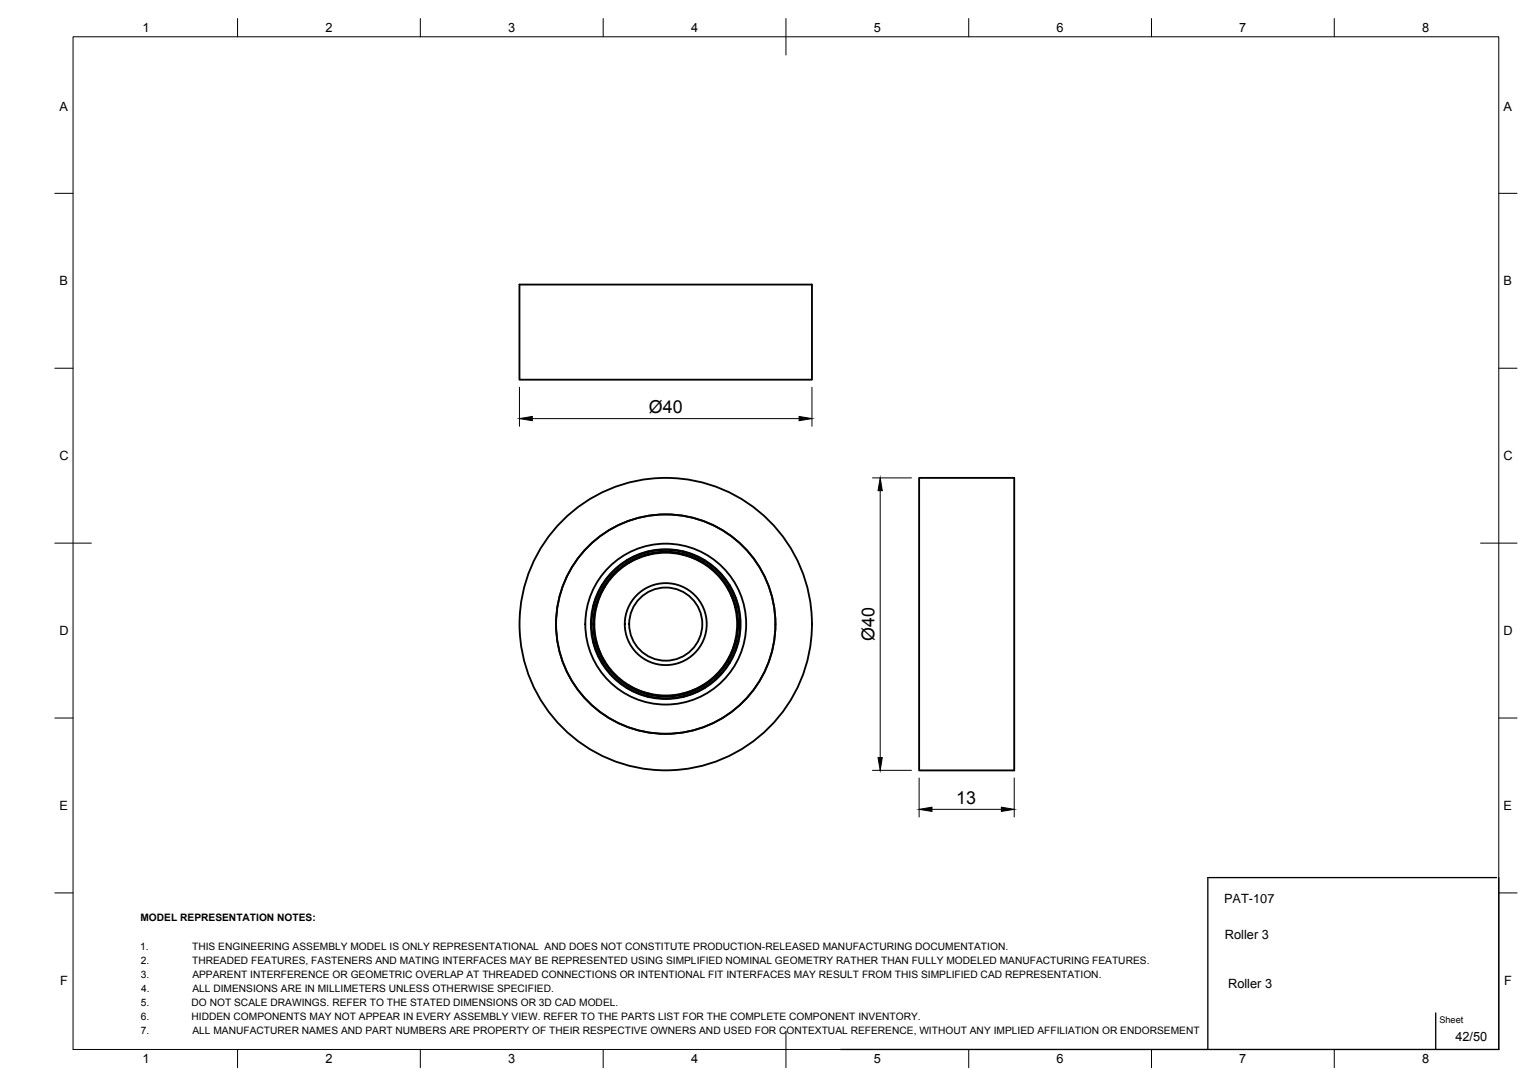
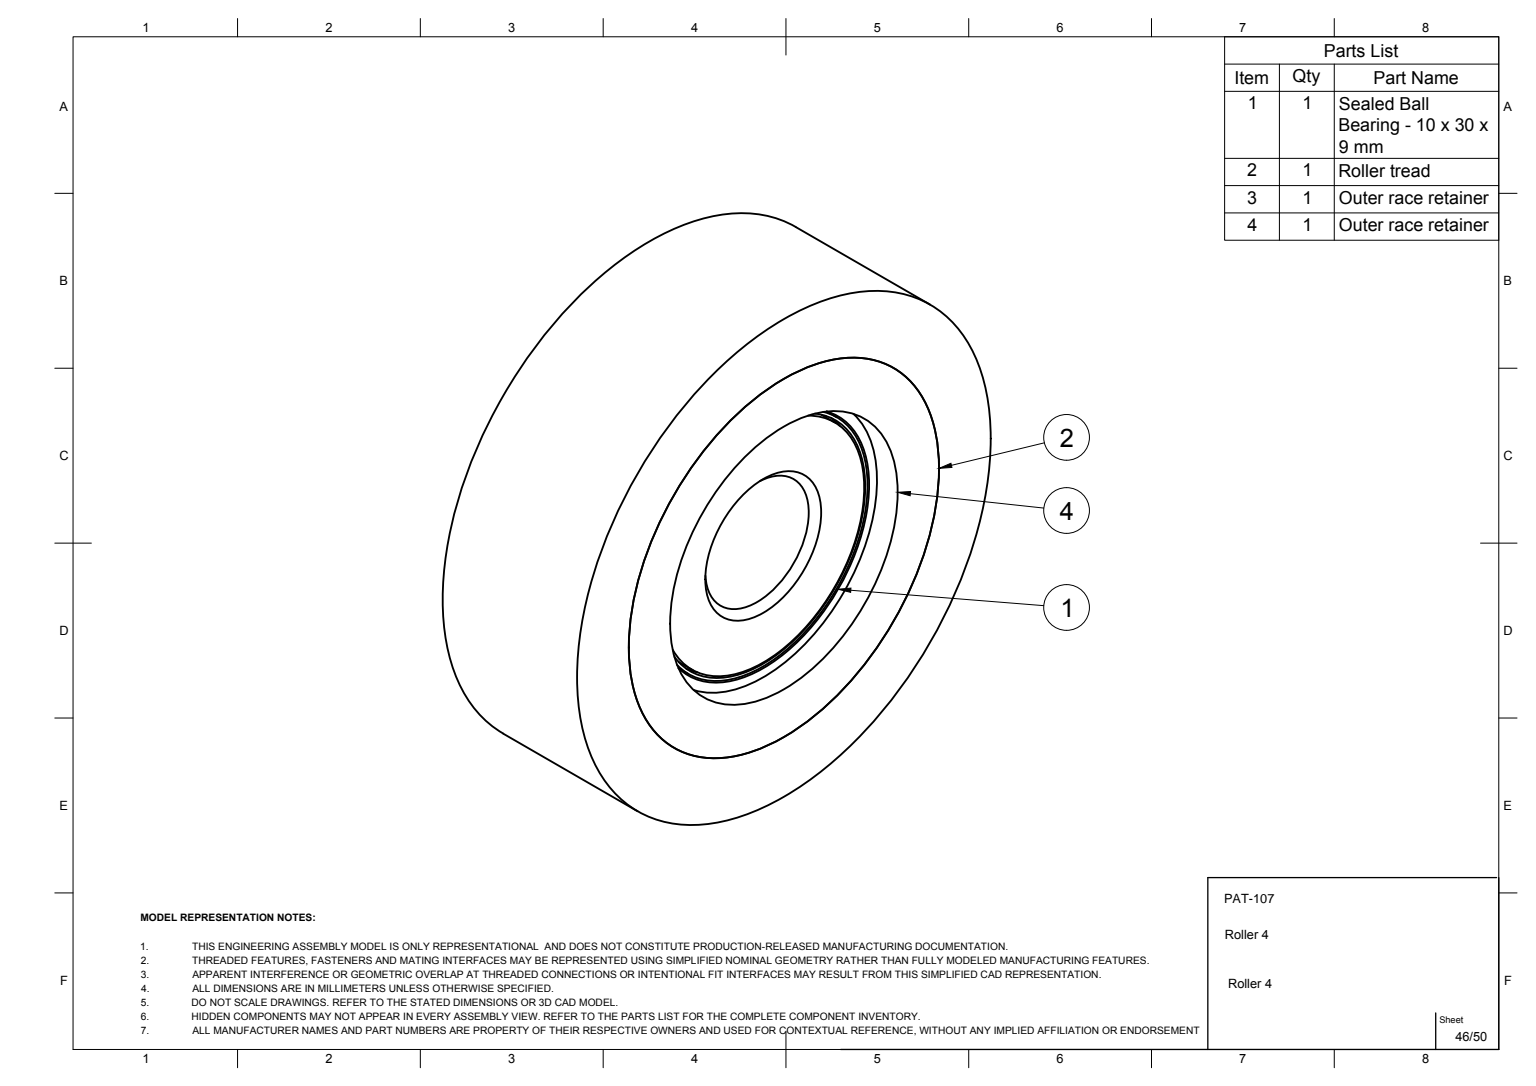
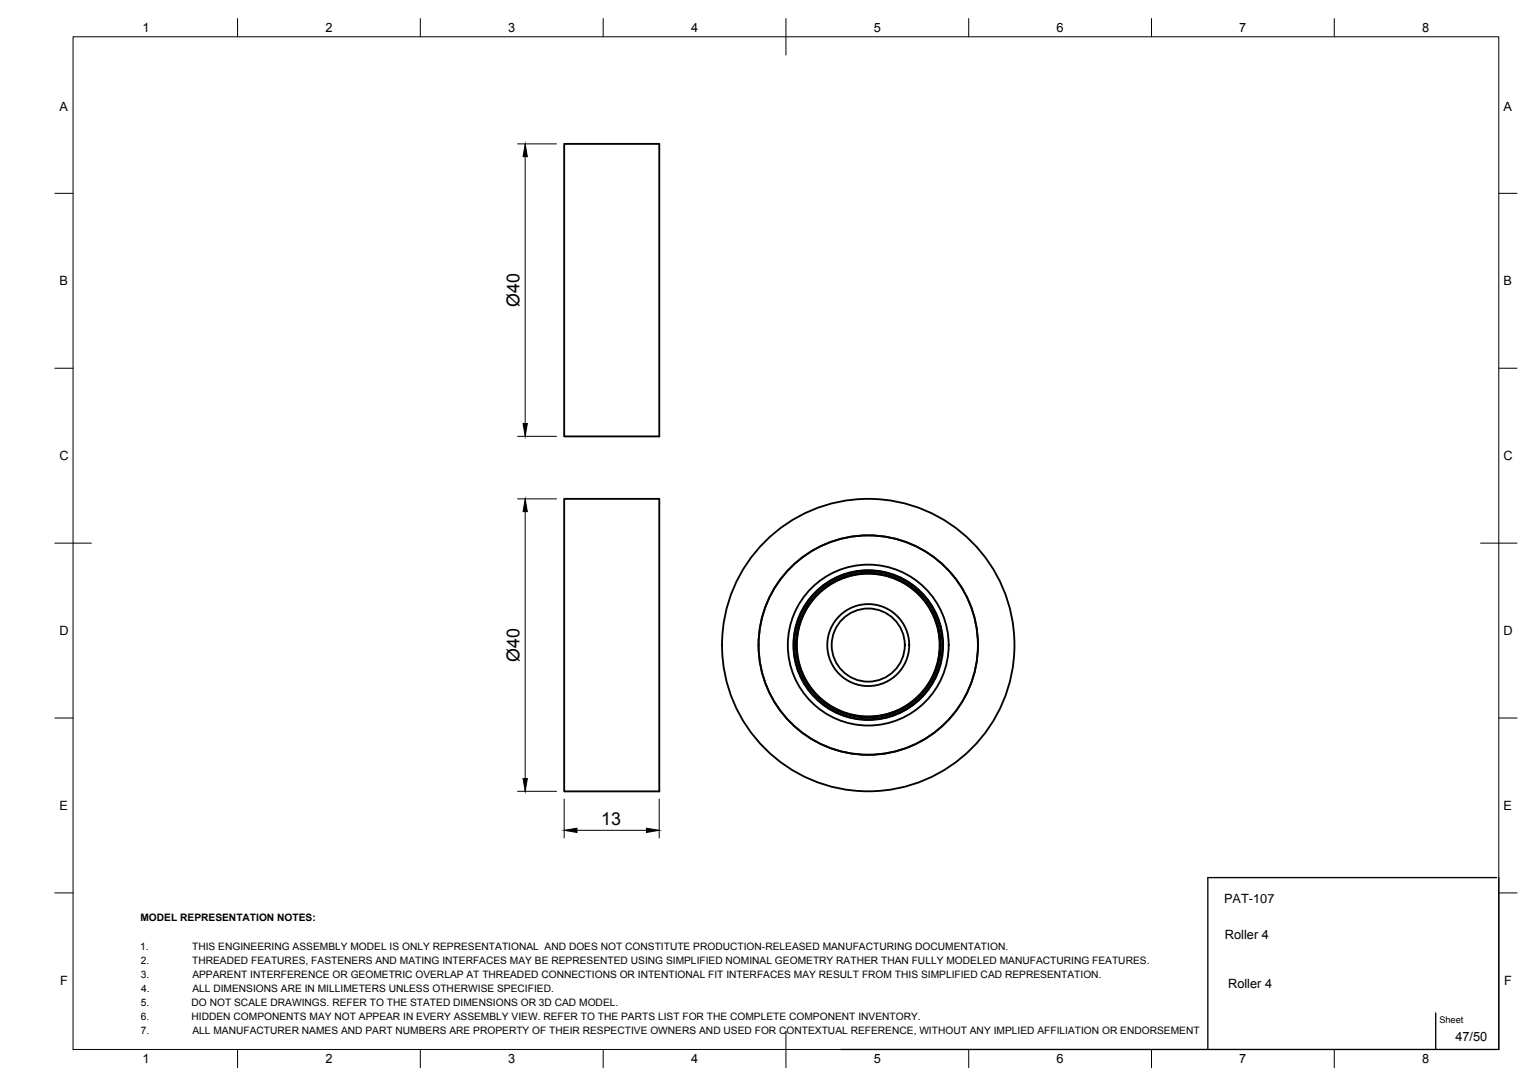
ISO-10303-21;
HEADER;
/* Generated by software containing ST-Developer
 * from STEP Tools, Inc. (www.steptools.com) 
 */

FILE_DESCRIPTION(
/* description */ ('Turntable on roller ring'),
/* implementation_level */ '2;1');

FILE_NAME(
/* name */ 'PAT-107',
/* time_stamp */ '2026-10-28T03:23:59-07:00',
/* author */ (''),
/* organization */ (''),
/* preprocessor_version */ 'ST-DEVELOPER v20.2',
/* originating_system */ 'Autodesk Translation Framework v15.17.0.0',
/* authorisation */ '');

FILE_SCHEMA (('AUTOMOTIVE_DESIGN { 1 0 10303 214 3 1 1 }'));
ENDSEC;

DATA;
#10=MECHANICAL_DESIGN_GEOMETRIC_PRESENTATION_REPRESENTATION('',(#617,#618,
#619,#620,#621,#622,#623,#624,#625,#626,#627,#628,#629,#630,#631,#632,#633,
#634,#635,#636,#637,#638,#639,#640,#641,#642,#643,#644,#645,#646,#647,#648,
#649,#650,#651,#652,#653,#654,#655,#656,#657,#658,#659,#660,#661,#662,#663,
#664,#665,#666,#667,#668,#669,#670,#671,#672,#673,#674,#675,#676,#677,#678,
#679,#680,#681,#682,#683,#684,#685,#686,#687,#688),#16281);
#11=ITEM_DEFINED_TRANSFORMATION($,$,#9231,#9369);
#12=ITEM_DEFINED_TRANSFORMATION($,$,#9251,#9370);
#13=ITEM_DEFINED_TRANSFORMATION($,$,#9271,#9371);
#14=ITEM_DEFINED_TRANSFORMATION($,$,#9290,#9372);
#15=ITEM_DEFINED_TRANSFORMATION($,$,#9352,#9373);
#16=ITEM_DEFINED_TRANSFORMATION($,$,#9042,#9494);
#17=ITEM_DEFINED_TRANSFORMATION($,$,#9109,#9495);
#18=ITEM_DEFINED_TRANSFORMATION($,$,#9181,#9496);
#19=ITEM_DEFINED_TRANSFORMATION($,$,#9206,#9497);
#20=ITEM_DEFINED_TRANSFORMATION($,$,#9206,#9498);
#21=ITEM_DEFINED_TRANSFORMATION($,$,#9206,#9499);
#22=ITEM_DEFINED_TRANSFORMATION($,$,#9206,#9500);
#23=ITEM_DEFINED_TRANSFORMATION($,$,#9230,#9501);
#24=ITEM_DEFINED_TRANSFORMATION($,$,#9468,#9502);
#25=ITEM_DEFINED_TRANSFORMATION($,$,#9468,#9503);
#26=ITEM_DEFINED_TRANSFORMATION($,$,#9468,#9504);
#27=ITEM_DEFINED_TRANSFORMATION($,$,#9468,#9505);
#28=ITEM_DEFINED_TRANSFORMATION($,$,#9374,#9506);
#29=ITEM_DEFINED_TRANSFORMATION($,$,#9381,#9507);
#30=ITEM_DEFINED_TRANSFORMATION($,$,#9389,#9525);
#31=ITEM_DEFINED_TRANSFORMATION($,$,#9411,#9526);
#32=ITEM_DEFINED_TRANSFORMATION($,$,#9453,#9527);
#33=ITEM_DEFINED_TRANSFORMATION($,$,#9468,#9528);
#34=ITEM_DEFINED_TRANSFORMATION($,$,#9468,#9529);
#35=ITEM_DEFINED_TRANSFORMATION($,$,#9468,#9530);
#36=ITEM_DEFINED_TRANSFORMATION($,$,#9508,#9531);
#37=ITEM_DEFINED_TRANSFORMATION($,$,#9533,#9888);
#38=ITEM_DEFINED_TRANSFORMATION($,$,#9568,#9889);
#39=ITEM_DEFINED_TRANSFORMATION($,$,#9582,#9890);
#40=ITEM_DEFINED_TRANSFORMATION($,$,#9591,#9891);
#41=ITEM_DEFINED_TRANSFORMATION($,$,#9600,#9892);
#42=ITEM_DEFINED_TRANSFORMATION($,$,#9840,#9893);
#43=ITEM_DEFINED_TRANSFORMATION($,$,#9840,#9894);
#44=ITEM_DEFINED_TRANSFORMATION($,$,#9840,#9895);
#45=ITEM_DEFINED_TRANSFORMATION($,$,#9840,#9896);
#46=ITEM_DEFINED_TRANSFORMATION($,$,#9864,#9897);
#47=ITEM_DEFINED_TRANSFORMATION($,$,#9610,#9898);
#48=ITEM_DEFINED_TRANSFORMATION($,$,#9645,#9899);
#49=ITEM_DEFINED_TRANSFORMATION($,$,#9659,#9900);
#50=ITEM_DEFINED_TRANSFORMATION($,$,#9668,#9901);
#51=ITEM_DEFINED_TRANSFORMATION($,$,#9677,#9902);
#52=ITEM_DEFINED_TRANSFORMATION($,$,#9840,#9903);
#53=ITEM_DEFINED_TRANSFORMATION($,$,#9840,#9904);
#54=ITEM_DEFINED_TRANSFORMATION($,$,#9840,#9905);
#55=ITEM_DEFINED_TRANSFORMATION($,$,#9840,#9906);
#56=ITEM_DEFINED_TRANSFORMATION($,$,#9864,#9907);
#57=ITEM_DEFINED_TRANSFORMATION($,$,#9687,#9908);
#58=ITEM_DEFINED_TRANSFORMATION($,$,#9722,#9909);
#59=ITEM_DEFINED_TRANSFORMATION($,$,#9736,#9910);
#60=ITEM_DEFINED_TRANSFORMATION($,$,#9745,#9911);
#61=ITEM_DEFINED_TRANSFORMATION($,$,#9754,#9912);
#62=ITEM_DEFINED_TRANSFORMATION($,$,#9840,#9913);
#63=ITEM_DEFINED_TRANSFORMATION($,$,#9840,#9914);
#64=ITEM_DEFINED_TRANSFORMATION($,$,#9840,#9915);
#65=ITEM_DEFINED_TRANSFORMATION($,$,#9840,#9916);
#66=ITEM_DEFINED_TRANSFORMATION($,$,#9864,#9917);
#67=ITEM_DEFINED_TRANSFORMATION($,$,#9764,#9918);
#68=ITEM_DEFINED_TRANSFORMATION($,$,#9799,#9919);
#69=ITEM_DEFINED_TRANSFORMATION($,$,#9813,#9920);
#70=ITEM_DEFINED_TRANSFORMATION($,$,#9822,#9921);
#71=ITEM_DEFINED_TRANSFORMATION($,$,#9831,#9922);
#72=ITEM_DEFINED_TRANSFORMATION($,$,#9840,#9923);
#73=ITEM_DEFINED_TRANSFORMATION($,$,#9840,#9924);
#74=ITEM_DEFINED_TRANSFORMATION($,$,#9840,#9925);
#75=ITEM_DEFINED_TRANSFORMATION($,$,#9840,#9926);
#76=ITEM_DEFINED_TRANSFORMATION($,$,#9864,#9927);
#77=ITEM_DEFINED_TRANSFORMATION($,$,#10041,#10169);
#78=ITEM_DEFINED_TRANSFORMATION($,$,#10061,#10170);
#79=ITEM_DEFINED_TRANSFORMATION($,$,#10081,#10171);
#80=ITEM_DEFINED_TRANSFORMATION($,$,#10098,#10172);
#81=ITEM_DEFINED_TRANSFORMATION($,$,#10152,#10173);
#82=ITEM_DEFINED_TRANSFORMATION($,$,#9929,#10174);
#83=ITEM_DEFINED_TRANSFORMATION($,$,#9938,#10175);
#84=ITEM_DEFINED_TRANSFORMATION($,$,#9947,#10176);
#85=ITEM_DEFINED_TRANSFORMATION($,$,#10040,#10177);
#86=ITEM_DEFINED_TRANSFORMATION($,$,#9957,#10178);
#87=ITEM_DEFINED_TRANSFORMATION($,$,#9966,#10179);
#88=ITEM_DEFINED_TRANSFORMATION($,$,#9975,#10180);
#89=ITEM_DEFINED_TRANSFORMATION($,$,#10040,#10181);
#90=ITEM_DEFINED_TRANSFORMATION($,$,#9985,#10182);
#91=ITEM_DEFINED_TRANSFORMATION($,$,#9994,#10183);
#92=ITEM_DEFINED_TRANSFORMATION($,$,#10003,#10184);
#93=ITEM_DEFINED_TRANSFORMATION($,$,#10040,#10185);
#94=ITEM_DEFINED_TRANSFORMATION($,$,#10013,#10186);
#95=ITEM_DEFINED_TRANSFORMATION($,$,#10022,#10187);
#96=ITEM_DEFINED_TRANSFORMATION($,$,#10031,#10188);
#97=ITEM_DEFINED_TRANSFORMATION($,$,#10040,#10189);
#98=ITEM_DEFINED_TRANSFORMATION($,$,#9041,#10190);
#99=ITEM_DEFINED_TRANSFORMATION($,$,#9388,#10191);
#100=ITEM_DEFINED_TRANSFORMATION($,$,#9532,#10192);
#101=ITEM_DEFINED_TRANSFORMATION($,$,#9609,#10193);
#102=ITEM_DEFINED_TRANSFORMATION($,$,#9686,#10194);
#103=ITEM_DEFINED_TRANSFORMATION($,$,#9763,#10195);
#104=ITEM_DEFINED_TRANSFORMATION($,$,#9928,#10196);
#105=ITEM_DEFINED_TRANSFORMATION($,$,#9956,#10197);
#106=ITEM_DEFINED_TRANSFORMATION($,$,#9984,#10198);
#107=ITEM_DEFINED_TRANSFORMATION($,$,#10012,#10199);
#108=(
REPRESENTATION_RELATIONSHIP($,$,#16526,#16525)
REPRESENTATION_RELATIONSHIP_WITH_TRANSFORMATION(#11)
SHAPE_REPRESENTATION_RELATIONSHIP()
);
#109=(
REPRESENTATION_RELATIONSHIP($,$,#16527,#16525)
REPRESENTATION_RELATIONSHIP_WITH_TRANSFORMATION(#12)
SHAPE_REPRESENTATION_RELATIONSHIP()
);
#110=(
REPRESENTATION_RELATIONSHIP($,$,#16528,#16525)
REPRESENTATION_RELATIONSHIP_WITH_TRANSFORMATION(#13)
SHAPE_REPRESENTATION_RELATIONSHIP()
);
#111=(
REPRESENTATION_RELATIONSHIP($,$,#16529,#16525)
REPRESENTATION_RELATIONSHIP_WITH_TRANSFORMATION(#14)
SHAPE_REPRESENTATION_RELATIONSHIP()
);
#112=(
REPRESENTATION_RELATIONSHIP($,$,#16530,#16525)
REPRESENTATION_RELATIONSHIP_WITH_TRANSFORMATION(#15)
SHAPE_REPRESENTATION_RELATIONSHIP()
);
#113=(
REPRESENTATION_RELATIONSHIP($,$,#16521,#16520)
REPRESENTATION_RELATIONSHIP_WITH_TRANSFORMATION(#16)
SHAPE_REPRESENTATION_RELATIONSHIP()
);
#114=(
REPRESENTATION_RELATIONSHIP($,$,#16522,#16520)
REPRESENTATION_RELATIONSHIP_WITH_TRANSFORMATION(#17)
SHAPE_REPRESENTATION_RELATIONSHIP()
);
#115=(
REPRESENTATION_RELATIONSHIP($,$,#16523,#16520)
REPRESENTATION_RELATIONSHIP_WITH_TRANSFORMATION(#18)
SHAPE_REPRESENTATION_RELATIONSHIP()
);
#116=(
REPRESENTATION_RELATIONSHIP($,$,#16524,#16520)
REPRESENTATION_RELATIONSHIP_WITH_TRANSFORMATION(#19)
SHAPE_REPRESENTATION_RELATIONSHIP()
);
#117=(
REPRESENTATION_RELATIONSHIP($,$,#16524,#16520)
REPRESENTATION_RELATIONSHIP_WITH_TRANSFORMATION(#20)
SHAPE_REPRESENTATION_RELATIONSHIP()
);
#118=(
REPRESENTATION_RELATIONSHIP($,$,#16524,#16520)
REPRESENTATION_RELATIONSHIP_WITH_TRANSFORMATION(#21)
SHAPE_REPRESENTATION_RELATIONSHIP()
);
#119=(
REPRESENTATION_RELATIONSHIP($,$,#16524,#16520)
REPRESENTATION_RELATIONSHIP_WITH_TRANSFORMATION(#22)
SHAPE_REPRESENTATION_RELATIONSHIP()
);
#120=(
REPRESENTATION_RELATIONSHIP($,$,#16525,#16520)
REPRESENTATION_RELATIONSHIP_WITH_TRANSFORMATION(#23)
SHAPE_REPRESENTATION_RELATIONSHIP()
);
#121=(
REPRESENTATION_RELATIONSHIP($,$,#16537,#16520)
REPRESENTATION_RELATIONSHIP_WITH_TRANSFORMATION(#24)
SHAPE_REPRESENTATION_RELATIONSHIP()
);
#122=(
REPRESENTATION_RELATIONSHIP($,$,#16537,#16520)
REPRESENTATION_RELATIONSHIP_WITH_TRANSFORMATION(#25)
SHAPE_REPRESENTATION_RELATIONSHIP()
);
#123=(
REPRESENTATION_RELATIONSHIP($,$,#16537,#16520)
REPRESENTATION_RELATIONSHIP_WITH_TRANSFORMATION(#26)
SHAPE_REPRESENTATION_RELATIONSHIP()
);
#124=(
REPRESENTATION_RELATIONSHIP($,$,#16537,#16520)
REPRESENTATION_RELATIONSHIP_WITH_TRANSFORMATION(#27)
SHAPE_REPRESENTATION_RELATIONSHIP()
);
#125=(
REPRESENTATION_RELATIONSHIP($,$,#16531,#16520)
REPRESENTATION_RELATIONSHIP_WITH_TRANSFORMATION(#28)
SHAPE_REPRESENTATION_RELATIONSHIP()
);
#126=(
REPRESENTATION_RELATIONSHIP($,$,#16532,#16520)
REPRESENTATION_RELATIONSHIP_WITH_TRANSFORMATION(#29)
SHAPE_REPRESENTATION_RELATIONSHIP()
);
#127=(
REPRESENTATION_RELATIONSHIP($,$,#16534,#16533)
REPRESENTATION_RELATIONSHIP_WITH_TRANSFORMATION(#30)
SHAPE_REPRESENTATION_RELATIONSHIP()
);
#128=(
REPRESENTATION_RELATIONSHIP($,$,#16535,#16533)
REPRESENTATION_RELATIONSHIP_WITH_TRANSFORMATION(#31)
SHAPE_REPRESENTATION_RELATIONSHIP()
);
#129=(
REPRESENTATION_RELATIONSHIP($,$,#16536,#16533)
REPRESENTATION_RELATIONSHIP_WITH_TRANSFORMATION(#32)
SHAPE_REPRESENTATION_RELATIONSHIP()
);
#130=(
REPRESENTATION_RELATIONSHIP($,$,#16537,#16533)
REPRESENTATION_RELATIONSHIP_WITH_TRANSFORMATION(#33)
SHAPE_REPRESENTATION_RELATIONSHIP()
);
#131=(
REPRESENTATION_RELATIONSHIP($,$,#16537,#16533)
REPRESENTATION_RELATIONSHIP_WITH_TRANSFORMATION(#34)
SHAPE_REPRESENTATION_RELATIONSHIP()
);
#132=(
REPRESENTATION_RELATIONSHIP($,$,#16537,#16533)
REPRESENTATION_RELATIONSHIP_WITH_TRANSFORMATION(#35)
SHAPE_REPRESENTATION_RELATIONSHIP()
);
#133=(
REPRESENTATION_RELATIONSHIP($,$,#16538,#16533)
REPRESENTATION_RELATIONSHIP_WITH_TRANSFORMATION(#36)
SHAPE_REPRESENTATION_RELATIONSHIP()
);
#134=(
REPRESENTATION_RELATIONSHIP($,$,#16540,#16539)
REPRESENTATION_RELATIONSHIP_WITH_TRANSFORMATION(#37)
SHAPE_REPRESENTATION_RELATIONSHIP()
);
#135=(
REPRESENTATION_RELATIONSHIP($,$,#16541,#16539)
REPRESENTATION_RELATIONSHIP_WITH_TRANSFORMATION(#38)
SHAPE_REPRESENTATION_RELATIONSHIP()
);
#136=(
REPRESENTATION_RELATIONSHIP($,$,#16542,#16539)
REPRESENTATION_RELATIONSHIP_WITH_TRANSFORMATION(#39)
SHAPE_REPRESENTATION_RELATIONSHIP()
);
#137=(
REPRESENTATION_RELATIONSHIP($,$,#16543,#16539)
REPRESENTATION_RELATIONSHIP_WITH_TRANSFORMATION(#40)
SHAPE_REPRESENTATION_RELATIONSHIP()
);
#138=(
REPRESENTATION_RELATIONSHIP($,$,#16544,#16539)
REPRESENTATION_RELATIONSHIP_WITH_TRANSFORMATION(#41)
SHAPE_REPRESENTATION_RELATIONSHIP()
);
#139=(
REPRESENTATION_RELATIONSHIP($,$,#16563,#16539)
REPRESENTATION_RELATIONSHIP_WITH_TRANSFORMATION(#42)
SHAPE_REPRESENTATION_RELATIONSHIP()
);
#140=(
REPRESENTATION_RELATIONSHIP($,$,#16563,#16539)
REPRESENTATION_RELATIONSHIP_WITH_TRANSFORMATION(#43)
SHAPE_REPRESENTATION_RELATIONSHIP()
);
#141=(
REPRESENTATION_RELATIONSHIP($,$,#16563,#16539)
REPRESENTATION_RELATIONSHIP_WITH_TRANSFORMATION(#44)
SHAPE_REPRESENTATION_RELATIONSHIP()
);
#142=(
REPRESENTATION_RELATIONSHIP($,$,#16563,#16539)
REPRESENTATION_RELATIONSHIP_WITH_TRANSFORMATION(#45)
SHAPE_REPRESENTATION_RELATIONSHIP()
);
#143=(
REPRESENTATION_RELATIONSHIP($,$,#16564,#16539)
REPRESENTATION_RELATIONSHIP_WITH_TRANSFORMATION(#46)
SHAPE_REPRESENTATION_RELATIONSHIP()
);
#144=(
REPRESENTATION_RELATIONSHIP($,$,#16546,#16545)
REPRESENTATION_RELATIONSHIP_WITH_TRANSFORMATION(#47)
SHAPE_REPRESENTATION_RELATIONSHIP()
);
#145=(
REPRESENTATION_RELATIONSHIP($,$,#16547,#16545)
REPRESENTATION_RELATIONSHIP_WITH_TRANSFORMATION(#48)
SHAPE_REPRESENTATION_RELATIONSHIP()
);
#146=(
REPRESENTATION_RELATIONSHIP($,$,#16548,#16545)
REPRESENTATION_RELATIONSHIP_WITH_TRANSFORMATION(#49)
SHAPE_REPRESENTATION_RELATIONSHIP()
);
#147=(
REPRESENTATION_RELATIONSHIP($,$,#16549,#16545)
REPRESENTATION_RELATIONSHIP_WITH_TRANSFORMATION(#50)
SHAPE_REPRESENTATION_RELATIONSHIP()
);
#148=(
REPRESENTATION_RELATIONSHIP($,$,#16550,#16545)
REPRESENTATION_RELATIONSHIP_WITH_TRANSFORMATION(#51)
SHAPE_REPRESENTATION_RELATIONSHIP()
);
#149=(
REPRESENTATION_RELATIONSHIP($,$,#16563,#16545)
REPRESENTATION_RELATIONSHIP_WITH_TRANSFORMATION(#52)
SHAPE_REPRESENTATION_RELATIONSHIP()
);
#150=(
REPRESENTATION_RELATIONSHIP($,$,#16563,#16545)
REPRESENTATION_RELATIONSHIP_WITH_TRANSFORMATION(#53)
SHAPE_REPRESENTATION_RELATIONSHIP()
);
#151=(
REPRESENTATION_RELATIONSHIP($,$,#16563,#16545)
REPRESENTATION_RELATIONSHIP_WITH_TRANSFORMATION(#54)
SHAPE_REPRESENTATION_RELATIONSHIP()
);
#152=(
REPRESENTATION_RELATIONSHIP($,$,#16563,#16545)
REPRESENTATION_RELATIONSHIP_WITH_TRANSFORMATION(#55)
SHAPE_REPRESENTATION_RELATIONSHIP()
);
#153=(
REPRESENTATION_RELATIONSHIP($,$,#16564,#16545)
REPRESENTATION_RELATIONSHIP_WITH_TRANSFORMATION(#56)
SHAPE_REPRESENTATION_RELATIONSHIP()
);
#154=(
REPRESENTATION_RELATIONSHIP($,$,#16552,#16551)
REPRESENTATION_RELATIONSHIP_WITH_TRANSFORMATION(#57)
SHAPE_REPRESENTATION_RELATIONSHIP()
);
#155=(
REPRESENTATION_RELATIONSHIP($,$,#16553,#16551)
REPRESENTATION_RELATIONSHIP_WITH_TRANSFORMATION(#58)
SHAPE_REPRESENTATION_RELATIONSHIP()
);
#156=(
REPRESENTATION_RELATIONSHIP($,$,#16554,#16551)
REPRESENTATION_RELATIONSHIP_WITH_TRANSFORMATION(#59)
SHAPE_REPRESENTATION_RELATIONSHIP()
);
#157=(
REPRESENTATION_RELATIONSHIP($,$,#16555,#16551)
REPRESENTATION_RELATIONSHIP_WITH_TRANSFORMATION(#60)
SHAPE_REPRESENTATION_RELATIONSHIP()
);
#158=(
REPRESENTATION_RELATIONSHIP($,$,#16556,#16551)
REPRESENTATION_RELATIONSHIP_WITH_TRANSFORMATION(#61)
SHAPE_REPRESENTATION_RELATIONSHIP()
);
#159=(
REPRESENTATION_RELATIONSHIP($,$,#16563,#16551)
REPRESENTATION_RELATIONSHIP_WITH_TRANSFORMATION(#62)
SHAPE_REPRESENTATION_RELATIONSHIP()
);
#160=(
REPRESENTATION_RELATIONSHIP($,$,#16563,#16551)
REPRESENTATION_RELATIONSHIP_WITH_TRANSFORMATION(#63)
SHAPE_REPRESENTATION_RELATIONSHIP()
);
#161=(
REPRESENTATION_RELATIONSHIP($,$,#16563,#16551)
REPRESENTATION_RELATIONSHIP_WITH_TRANSFORMATION(#64)
SHAPE_REPRESENTATION_RELATIONSHIP()
);
#162=(
REPRESENTATION_RELATIONSHIP($,$,#16563,#16551)
REPRESENTATION_RELATIONSHIP_WITH_TRANSFORMATION(#65)
SHAPE_REPRESENTATION_RELATIONSHIP()
);
#163=(
REPRESENTATION_RELATIONSHIP($,$,#16564,#16551)
REPRESENTATION_RELATIONSHIP_WITH_TRANSFORMATION(#66)
SHAPE_REPRESENTATION_RELATIONSHIP()
);
#164=(
REPRESENTATION_RELATIONSHIP($,$,#16558,#16557)
REPRESENTATION_RELATIONSHIP_WITH_TRANSFORMATION(#67)
SHAPE_REPRESENTATION_RELATIONSHIP()
);
#165=(
REPRESENTATION_RELATIONSHIP($,$,#16559,#16557)
REPRESENTATION_RELATIONSHIP_WITH_TRANSFORMATION(#68)
SHAPE_REPRESENTATION_RELATIONSHIP()
);
#166=(
REPRESENTATION_RELATIONSHIP($,$,#16560,#16557)
REPRESENTATION_RELATIONSHIP_WITH_TRANSFORMATION(#69)
SHAPE_REPRESENTATION_RELATIONSHIP()
);
#167=(
REPRESENTATION_RELATIONSHIP($,$,#16561,#16557)
REPRESENTATION_RELATIONSHIP_WITH_TRANSFORMATION(#70)
SHAPE_REPRESENTATION_RELATIONSHIP()
);
#168=(
REPRESENTATION_RELATIONSHIP($,$,#16562,#16557)
REPRESENTATION_RELATIONSHIP_WITH_TRANSFORMATION(#71)
SHAPE_REPRESENTATION_RELATIONSHIP()
);
#169=(
REPRESENTATION_RELATIONSHIP($,$,#16563,#16557)
REPRESENTATION_RELATIONSHIP_WITH_TRANSFORMATION(#72)
SHAPE_REPRESENTATION_RELATIONSHIP()
);
#170=(
REPRESENTATION_RELATIONSHIP($,$,#16563,#16557)
REPRESENTATION_RELATIONSHIP_WITH_TRANSFORMATION(#73)
SHAPE_REPRESENTATION_RELATIONSHIP()
);
#171=(
REPRESENTATION_RELATIONSHIP($,$,#16563,#16557)
REPRESENTATION_RELATIONSHIP_WITH_TRANSFORMATION(#74)
SHAPE_REPRESENTATION_RELATIONSHIP()
);
#172=(
REPRESENTATION_RELATIONSHIP($,$,#16563,#16557)
REPRESENTATION_RELATIONSHIP_WITH_TRANSFORMATION(#75)
SHAPE_REPRESENTATION_RELATIONSHIP()
);
#173=(
REPRESENTATION_RELATIONSHIP($,$,#16564,#16557)
REPRESENTATION_RELATIONSHIP_WITH_TRANSFORMATION(#76)
SHAPE_REPRESENTATION_RELATIONSHIP()
);
#174=(
REPRESENTATION_RELATIONSHIP($,$,#16582,#16581)
REPRESENTATION_RELATIONSHIP_WITH_TRANSFORMATION(#77)
SHAPE_REPRESENTATION_RELATIONSHIP()
);
#175=(
REPRESENTATION_RELATIONSHIP($,$,#16583,#16581)
REPRESENTATION_RELATIONSHIP_WITH_TRANSFORMATION(#78)
SHAPE_REPRESENTATION_RELATIONSHIP()
);
#176=(
REPRESENTATION_RELATIONSHIP($,$,#16584,#16581)
REPRESENTATION_RELATIONSHIP_WITH_TRANSFORMATION(#79)
SHAPE_REPRESENTATION_RELATIONSHIP()
);
#177=(
REPRESENTATION_RELATIONSHIP($,$,#16585,#16581)
REPRESENTATION_RELATIONSHIP_WITH_TRANSFORMATION(#80)
SHAPE_REPRESENTATION_RELATIONSHIP()
);
#178=(
REPRESENTATION_RELATIONSHIP($,$,#16586,#16581)
REPRESENTATION_RELATIONSHIP_WITH_TRANSFORMATION(#81)
SHAPE_REPRESENTATION_RELATIONSHIP()
);
#179=(
REPRESENTATION_RELATIONSHIP($,$,#16566,#16565)
REPRESENTATION_RELATIONSHIP_WITH_TRANSFORMATION(#82)
SHAPE_REPRESENTATION_RELATIONSHIP()
);
#180=(
REPRESENTATION_RELATIONSHIP($,$,#16567,#16565)
REPRESENTATION_RELATIONSHIP_WITH_TRANSFORMATION(#83)
SHAPE_REPRESENTATION_RELATIONSHIP()
);
#181=(
REPRESENTATION_RELATIONSHIP($,$,#16568,#16565)
REPRESENTATION_RELATIONSHIP_WITH_TRANSFORMATION(#84)
SHAPE_REPRESENTATION_RELATIONSHIP()
);
#182=(
REPRESENTATION_RELATIONSHIP($,$,#16581,#16565)
REPRESENTATION_RELATIONSHIP_WITH_TRANSFORMATION(#85)
SHAPE_REPRESENTATION_RELATIONSHIP()
);
#183=(
REPRESENTATION_RELATIONSHIP($,$,#16570,#16569)
REPRESENTATION_RELATIONSHIP_WITH_TRANSFORMATION(#86)
SHAPE_REPRESENTATION_RELATIONSHIP()
);
#184=(
REPRESENTATION_RELATIONSHIP($,$,#16571,#16569)
REPRESENTATION_RELATIONSHIP_WITH_TRANSFORMATION(#87)
SHAPE_REPRESENTATION_RELATIONSHIP()
);
#185=(
REPRESENTATION_RELATIONSHIP($,$,#16572,#16569)
REPRESENTATION_RELATIONSHIP_WITH_TRANSFORMATION(#88)
SHAPE_REPRESENTATION_RELATIONSHIP()
);
#186=(
REPRESENTATION_RELATIONSHIP($,$,#16581,#16569)
REPRESENTATION_RELATIONSHIP_WITH_TRANSFORMATION(#89)
SHAPE_REPRESENTATION_RELATIONSHIP()
);
#187=(
REPRESENTATION_RELATIONSHIP($,$,#16574,#16573)
REPRESENTATION_RELATIONSHIP_WITH_TRANSFORMATION(#90)
SHAPE_REPRESENTATION_RELATIONSHIP()
);
#188=(
REPRESENTATION_RELATIONSHIP($,$,#16575,#16573)
REPRESENTATION_RELATIONSHIP_WITH_TRANSFORMATION(#91)
SHAPE_REPRESENTATION_RELATIONSHIP()
);
#189=(
REPRESENTATION_RELATIONSHIP($,$,#16576,#16573)
REPRESENTATION_RELATIONSHIP_WITH_TRANSFORMATION(#92)
SHAPE_REPRESENTATION_RELATIONSHIP()
);
#190=(
REPRESENTATION_RELATIONSHIP($,$,#16581,#16573)
REPRESENTATION_RELATIONSHIP_WITH_TRANSFORMATION(#93)
SHAPE_REPRESENTATION_RELATIONSHIP()
);
#191=(
REPRESENTATION_RELATIONSHIP($,$,#16578,#16577)
REPRESENTATION_RELATIONSHIP_WITH_TRANSFORMATION(#94)
SHAPE_REPRESENTATION_RELATIONSHIP()
);
#192=(
REPRESENTATION_RELATIONSHIP($,$,#16579,#16577)
REPRESENTATION_RELATIONSHIP_WITH_TRANSFORMATION(#95)
SHAPE_REPRESENTATION_RELATIONSHIP()
);
#193=(
REPRESENTATION_RELATIONSHIP($,$,#16580,#16577)
REPRESENTATION_RELATIONSHIP_WITH_TRANSFORMATION(#96)
SHAPE_REPRESENTATION_RELATIONSHIP()
);
#194=(
REPRESENTATION_RELATIONSHIP($,$,#16581,#16577)
REPRESENTATION_RELATIONSHIP_WITH_TRANSFORMATION(#97)
SHAPE_REPRESENTATION_RELATIONSHIP()
);
#195=(
REPRESENTATION_RELATIONSHIP($,$,#16520,#16519)
REPRESENTATION_RELATIONSHIP_WITH_TRANSFORMATION(#98)
SHAPE_REPRESENTATION_RELATIONSHIP()
);
#196=(
REPRESENTATION_RELATIONSHIP($,$,#16533,#16519)
REPRESENTATION_RELATIONSHIP_WITH_TRANSFORMATION(#99)
SHAPE_REPRESENTATION_RELATIONSHIP()
);
#197=(
REPRESENTATION_RELATIONSHIP($,$,#16539,#16519)
REPRESENTATION_RELATIONSHIP_WITH_TRANSFORMATION(#100)
SHAPE_REPRESENTATION_RELATIONSHIP()
);
#198=(
REPRESENTATION_RELATIONSHIP($,$,#16545,#16519)
REPRESENTATION_RELATIONSHIP_WITH_TRANSFORMATION(#101)
SHAPE_REPRESENTATION_RELATIONSHIP()
);
#199=(
REPRESENTATION_RELATIONSHIP($,$,#16551,#16519)
REPRESENTATION_RELATIONSHIP_WITH_TRANSFORMATION(#102)
SHAPE_REPRESENTATION_RELATIONSHIP()
);
#200=(
REPRESENTATION_RELATIONSHIP($,$,#16557,#16519)
REPRESENTATION_RELATIONSHIP_WITH_TRANSFORMATION(#103)
SHAPE_REPRESENTATION_RELATIONSHIP()
);
#201=(
REPRESENTATION_RELATIONSHIP($,$,#16565,#16519)
REPRESENTATION_RELATIONSHIP_WITH_TRANSFORMATION(#104)
SHAPE_REPRESENTATION_RELATIONSHIP()
);
#202=(
REPRESENTATION_RELATIONSHIP($,$,#16569,#16519)
REPRESENTATION_RELATIONSHIP_WITH_TRANSFORMATION(#105)
SHAPE_REPRESENTATION_RELATIONSHIP()
);
#203=(
REPRESENTATION_RELATIONSHIP($,$,#16573,#16519)
REPRESENTATION_RELATIONSHIP_WITH_TRANSFORMATION(#106)
SHAPE_REPRESENTATION_RELATIONSHIP()
);
#204=(
REPRESENTATION_RELATIONSHIP($,$,#16577,#16519)
REPRESENTATION_RELATIONSHIP_WITH_TRANSFORMATION(#107)
SHAPE_REPRESENTATION_RELATIONSHIP()
);
#205=CONTEXT_DEPENDENT_SHAPE_REPRESENTATION(#108,#16366);
#206=CONTEXT_DEPENDENT_SHAPE_REPRESENTATION(#109,#16367);
#207=CONTEXT_DEPENDENT_SHAPE_REPRESENTATION(#110,#16368);
#208=CONTEXT_DEPENDENT_SHAPE_REPRESENTATION(#111,#16369);
#209=CONTEXT_DEPENDENT_SHAPE_REPRESENTATION(#112,#16370);
#210=CONTEXT_DEPENDENT_SHAPE_REPRESENTATION(#113,#16378);
#211=CONTEXT_DEPENDENT_SHAPE_REPRESENTATION(#114,#16379);
#212=CONTEXT_DEPENDENT_SHAPE_REPRESENTATION(#115,#16380);
#213=CONTEXT_DEPENDENT_SHAPE_REPRESENTATION(#116,#16381);
#214=CONTEXT_DEPENDENT_SHAPE_REPRESENTATION(#117,#16382);
#215=CONTEXT_DEPENDENT_SHAPE_REPRESENTATION(#118,#16383);
#216=CONTEXT_DEPENDENT_SHAPE_REPRESENTATION(#119,#16384);
#217=CONTEXT_DEPENDENT_SHAPE_REPRESENTATION(#120,#16385);
#218=CONTEXT_DEPENDENT_SHAPE_REPRESENTATION(#121,#16386);
#219=CONTEXT_DEPENDENT_SHAPE_REPRESENTATION(#122,#16387);
#220=CONTEXT_DEPENDENT_SHAPE_REPRESENTATION(#123,#16388);
#221=CONTEXT_DEPENDENT_SHAPE_REPRESENTATION(#124,#16389);
#222=CONTEXT_DEPENDENT_SHAPE_REPRESENTATION(#125,#16390);
#223=CONTEXT_DEPENDENT_SHAPE_REPRESENTATION(#126,#16391);
#224=CONTEXT_DEPENDENT_SHAPE_REPRESENTATION(#127,#16393);
#225=CONTEXT_DEPENDENT_SHAPE_REPRESENTATION(#128,#16394);
#226=CONTEXT_DEPENDENT_SHAPE_REPRESENTATION(#129,#16395);
#227=CONTEXT_DEPENDENT_SHAPE_REPRESENTATION(#130,#16396);
#228=CONTEXT_DEPENDENT_SHAPE_REPRESENTATION(#131,#16397);
#229=CONTEXT_DEPENDENT_SHAPE_REPRESENTATION(#132,#16398);
#230=CONTEXT_DEPENDENT_SHAPE_REPRESENTATION(#133,#16399);
#231=CONTEXT_DEPENDENT_SHAPE_REPRESENTATION(#134,#16426);
#232=CONTEXT_DEPENDENT_SHAPE_REPRESENTATION(#135,#16427);
#233=CONTEXT_DEPENDENT_SHAPE_REPRESENTATION(#136,#16428);
#234=CONTEXT_DEPENDENT_SHAPE_REPRESENTATION(#137,#16429);
#235=CONTEXT_DEPENDENT_SHAPE_REPRESENTATION(#138,#16430);
#236=CONTEXT_DEPENDENT_SHAPE_REPRESENTATION(#139,#16431);
#237=CONTEXT_DEPENDENT_SHAPE_REPRESENTATION(#140,#16432);
#238=CONTEXT_DEPENDENT_SHAPE_REPRESENTATION(#141,#16433);
#239=CONTEXT_DEPENDENT_SHAPE_REPRESENTATION(#142,#16434);
#240=CONTEXT_DEPENDENT_SHAPE_REPRESENTATION(#143,#16435);
#241=CONTEXT_DEPENDENT_SHAPE_REPRESENTATION(#144,#16436);
#242=CONTEXT_DEPENDENT_SHAPE_REPRESENTATION(#145,#16437);
#243=CONTEXT_DEPENDENT_SHAPE_REPRESENTATION(#146,#16438);
#244=CONTEXT_DEPENDENT_SHAPE_REPRESENTATION(#147,#16439);
#245=CONTEXT_DEPENDENT_SHAPE_REPRESENTATION(#148,#16440);
#246=CONTEXT_DEPENDENT_SHAPE_REPRESENTATION(#149,#16441);
#247=CONTEXT_DEPENDENT_SHAPE_REPRESENTATION(#150,#16442);
#248=CONTEXT_DEPENDENT_SHAPE_REPRESENTATION(#151,#16443);
#249=CONTEXT_DEPENDENT_SHAPE_REPRESENTATION(#152,#16444);
#250=CONTEXT_DEPENDENT_SHAPE_REPRESENTATION(#153,#16445);
#251=CONTEXT_DEPENDENT_SHAPE_REPRESENTATION(#154,#16446);
#252=CONTEXT_DEPENDENT_SHAPE_REPRESENTATION(#155,#16447);
#253=CONTEXT_DEPENDENT_SHAPE_REPRESENTATION(#156,#16448);
#254=CONTEXT_DEPENDENT_SHAPE_REPRESENTATION(#157,#16449);
#255=CONTEXT_DEPENDENT_SHAPE_REPRESENTATION(#158,#16450);
#256=CONTEXT_DEPENDENT_SHAPE_REPRESENTATION(#159,#16451);
#257=CONTEXT_DEPENDENT_SHAPE_REPRESENTATION(#160,#16452);
#258=CONTEXT_DEPENDENT_SHAPE_REPRESENTATION(#161,#16453);
#259=CONTEXT_DEPENDENT_SHAPE_REPRESENTATION(#162,#16454);
#260=CONTEXT_DEPENDENT_SHAPE_REPRESENTATION(#163,#16455);
#261=CONTEXT_DEPENDENT_SHAPE_REPRESENTATION(#164,#16456);
#262=CONTEXT_DEPENDENT_SHAPE_REPRESENTATION(#165,#16457);
#263=CONTEXT_DEPENDENT_SHAPE_REPRESENTATION(#166,#16458);
#264=CONTEXT_DEPENDENT_SHAPE_REPRESENTATION(#167,#16459);
#265=CONTEXT_DEPENDENT_SHAPE_REPRESENTATION(#168,#16460);
#266=CONTEXT_DEPENDENT_SHAPE_REPRESENTATION(#169,#16461);
#267=CONTEXT_DEPENDENT_SHAPE_REPRESENTATION(#170,#16462);
#268=CONTEXT_DEPENDENT_SHAPE_REPRESENTATION(#171,#16463);
#269=CONTEXT_DEPENDENT_SHAPE_REPRESENTATION(#172,#16464);
#270=CONTEXT_DEPENDENT_SHAPE_REPRESENTATION(#173,#16465);
#271=CONTEXT_DEPENDENT_SHAPE_REPRESENTATION(#174,#16488);
#272=CONTEXT_DEPENDENT_SHAPE_REPRESENTATION(#175,#16489);
#273=CONTEXT_DEPENDENT_SHAPE_REPRESENTATION(#176,#16490);
#274=CONTEXT_DEPENDENT_SHAPE_REPRESENTATION(#177,#16491);
#275=CONTEXT_DEPENDENT_SHAPE_REPRESENTATION(#178,#16492);
#276=CONTEXT_DEPENDENT_SHAPE_REPRESENTATION(#179,#16493);
#277=CONTEXT_DEPENDENT_SHAPE_REPRESENTATION(#180,#16494);
#278=CONTEXT_DEPENDENT_SHAPE_REPRESENTATION(#181,#16495);
#279=CONTEXT_DEPENDENT_SHAPE_REPRESENTATION(#182,#16496);
#280=CONTEXT_DEPENDENT_SHAPE_REPRESENTATION(#183,#16497);
#281=CONTEXT_DEPENDENT_SHAPE_REPRESENTATION(#184,#16498);
#282=CONTEXT_DEPENDENT_SHAPE_REPRESENTATION(#185,#16499);
#283=CONTEXT_DEPENDENT_SHAPE_REPRESENTATION(#186,#16500);
#284=CONTEXT_DEPENDENT_SHAPE_REPRESENTATION(#187,#16501);
#285=CONTEXT_DEPENDENT_SHAPE_REPRESENTATION(#188,#16502);
#286=CONTEXT_DEPENDENT_SHAPE_REPRESENTATION(#189,#16503);
#287=CONTEXT_DEPENDENT_SHAPE_REPRESENTATION(#190,#16504);
#288=CONTEXT_DEPENDENT_SHAPE_REPRESENTATION(#191,#16505);
#289=CONTEXT_DEPENDENT_SHAPE_REPRESENTATION(#192,#16506);
#290=CONTEXT_DEPENDENT_SHAPE_REPRESENTATION(#193,#16507);
#291=CONTEXT_DEPENDENT_SHAPE_REPRESENTATION(#194,#16508);
#292=CONTEXT_DEPENDENT_SHAPE_REPRESENTATION(#195,#16509);
#293=CONTEXT_DEPENDENT_SHAPE_REPRESENTATION(#196,#16510);
#294=CONTEXT_DEPENDENT_SHAPE_REPRESENTATION(#197,#16511);
#295=CONTEXT_DEPENDENT_SHAPE_REPRESENTATION(#198,#16512);
#296=CONTEXT_DEPENDENT_SHAPE_REPRESENTATION(#199,#16513);
#297=CONTEXT_DEPENDENT_SHAPE_REPRESENTATION(#200,#16514);
#298=CONTEXT_DEPENDENT_SHAPE_REPRESENTATION(#201,#16515);
#299=CONTEXT_DEPENDENT_SHAPE_REPRESENTATION(#202,#16516);
#300=CONTEXT_DEPENDENT_SHAPE_REPRESENTATION(#203,#16517);
#301=CONTEXT_DEPENDENT_SHAPE_REPRESENTATION(#204,#16518);
#302=NEXT_ASSEMBLY_USAGE_OCCURRENCE('Inner ring:1','Inner ring:1',
'Inner ring:1',#16594,#16595,'Inner ring:1');
#303=NEXT_ASSEMBLY_USAGE_OCCURRENCE('Outer ring:1','Outer ring:1',
'Outer ring:1',#16594,#16596,'Outer ring:1');
#304=NEXT_ASSEMBLY_USAGE_OCCURRENCE('Balls:1','Balls:1','Balls:1',#16594,
#16597,'Balls:1');
#305=NEXT_ASSEMBLY_USAGE_OCCURRENCE('Cage:1','Cage:1','Cage:1',#16594,#16598,
'Cage:1');
#306=NEXT_ASSEMBLY_USAGE_OCCURRENCE('Seals 2RS:1','Seals 2RS:1',
'Seals 2RS:1',#16594,#16599,'Seals 2RS:1');
#307=NEXT_ASSEMBLY_USAGE_OCCURRENCE('Base:1','Base:1','Base:1',#16589,#16590,
'Base:1');
#308=NEXT_ASSEMBLY_USAGE_OCCURRENCE('Centre housing:1',
'Centre housing:1','Centre housing:1',#16589,#16591,'Centre housing:1');
#309=NEXT_ASSEMBLY_USAGE_OCCURRENCE('Bearing cap:1','Bearing cap:1',
'Bearing cap:1',#16589,#16592,'Bearing cap:1');
#310=NEXT_ASSEMBLY_USAGE_OCCURRENCE('M6x18 mounting screw:2',
'M6x18 mounting screw:2','M6x18 mounting screw:2',#16589,#16593,
'M6x18 mounting screw:2');
#311=NEXT_ASSEMBLY_USAGE_OCCURRENCE('M6x18 mounting screw:3',
'M6x18 mounting screw:3','M6x18 mounting screw:3',#16589,#16593,
'M6x18 mounting screw:3');
#312=NEXT_ASSEMBLY_USAGE_OCCURRENCE('M6x18 mounting screw:4',
'M6x18 mounting screw:4','M6x18 mounting screw:4',#16589,#16593,
'M6x18 mounting screw:4');
#313=NEXT_ASSEMBLY_USAGE_OCCURRENCE('M6x18 mounting screw:5',
'M6x18 mounting screw:5','M6x18 mounting screw:5',#16589,#16593,
'M6x18 mounting screw:5');
#314=NEXT_ASSEMBLY_USAGE_OCCURRENCE(
'Sealed Ball Bearing - 25 x 52 x 15 mm:2',
'Sealed Ball Bearing - 25 x 52 x 15 mm:2',
'Sealed Ball Bearing - 25 x 52 x 15 mm:2',#16589,#16594,
'Sealed Ball Bearing - 25 x 52 x 15 mm:2');
#315=NEXT_ASSEMBLY_USAGE_OCCURRENCE('Cap Screw - M4x16:2',
'Cap Screw - M4x16:2','Cap Screw - M4x16:2',#16589,#16606,
'Cap Screw - M4x16:2');
#316=NEXT_ASSEMBLY_USAGE_OCCURRENCE('Cap Screw - M4x16:3',
'Cap Screw - M4x16:3','Cap Screw - M4x16:3',#16589,#16606,
'Cap Screw - M4x16:3');
#317=NEXT_ASSEMBLY_USAGE_OCCURRENCE('Cap Screw - M4x16:4',
'Cap Screw - M4x16:4','Cap Screw - M4x16:4',#16589,#16606,
'Cap Screw - M4x16:4');
#318=NEXT_ASSEMBLY_USAGE_OCCURRENCE('Cap Screw - M4x16:5',
'Cap Screw - M4x16:5','Cap Screw - M4x16:5',#16589,#16606,
'Cap Screw - M4x16:5');
#319=NEXT_ASSEMBLY_USAGE_OCCURRENCE('Bonded foot:1','Bonded foot:1',
'Bonded foot:1',#16589,#16600,'Bonded foot:1');
#320=NEXT_ASSEMBLY_USAGE_OCCURRENCE('Bonded foot (1):1',
'Bonded foot (1):1','Bonded foot (1):1',#16589,#16601,
'Bonded foot (1):1');
#321=NEXT_ASSEMBLY_USAGE_OCCURRENCE('Centre spindle:1',
'Centre spindle:1','Centre spindle:1',#16602,#16603,'Centre spindle:1');
#322=NEXT_ASSEMBLY_USAGE_OCCURRENCE('Table disc:1','Table disc:1',
'Table disc:1',#16602,#16604,'Table disc:1');
#323=NEXT_ASSEMBLY_USAGE_OCCURRENCE('Retention collar:1',
'Retention collar:1','Retention collar:1',#16602,#16605,
'Retention collar:1');
#324=NEXT_ASSEMBLY_USAGE_OCCURRENCE('Cap Screw - M4x16:6',
'Cap Screw - M4x16:6','Cap Screw - M4x16:6',#16602,#16606,
'Cap Screw - M4x16:6');
#325=NEXT_ASSEMBLY_USAGE_OCCURRENCE('Cap Screw - M4x16:7',
'Cap Screw - M4x16:7','Cap Screw - M4x16:7',#16602,#16606,
'Cap Screw - M4x16:7');
#326=NEXT_ASSEMBLY_USAGE_OCCURRENCE('Cap Screw - M4x16:8',
'Cap Screw - M4x16:8','Cap Screw - M4x16:8',#16602,#16606,
'Cap Screw - M4x16:8');
#327=NEXT_ASSEMBLY_USAGE_OCCURRENCE('Socket Set Screw - M5x8:2',
'Socket Set Screw - M5x8:2','Socket Set Screw - M5x8:2',#16602,#16607,
'Socket Set Screw - M5x8:2');
#328=NEXT_ASSEMBLY_USAGE_OCCURRENCE('Roller bracket:1',
'Roller bracket:1','Roller bracket:1',#16608,#16609,'Roller bracket:1');
#329=NEXT_ASSEMBLY_USAGE_OCCURRENCE('Roller axle:1','Roller axle:1',
'Roller axle:1',#16608,#16610,'Roller axle:1');
#330=NEXT_ASSEMBLY_USAGE_OCCURRENCE('Inner race spacer:1',
'Inner race spacer:1','Inner race spacer:1',#16608,#16611,
'Inner race spacer:1');
#331=NEXT_ASSEMBLY_USAGE_OCCURRENCE('Inner race spacer (1):1',
'Inner race spacer (1):1','Inner race spacer (1):1',#16608,#16612,
'Inner race spacer (1):1');
#332=NEXT_ASSEMBLY_USAGE_OCCURRENCE('Axle keeper:1','Axle keeper:1',
'Axle keeper:1',#16608,#16613,'Axle keeper:1');
#333=NEXT_ASSEMBLY_USAGE_OCCURRENCE('M5x14 Cap Screw:2',
'M5x14 Cap Screw:2','M5x14 Cap Screw:2',#16608,#16632,
'M5x14 Cap Screw:2');
#334=NEXT_ASSEMBLY_USAGE_OCCURRENCE('M5x14 Cap Screw:3',
'M5x14 Cap Screw:3','M5x14 Cap Screw:3',#16608,#16632,
'M5x14 Cap Screw:3');
#335=NEXT_ASSEMBLY_USAGE_OCCURRENCE('M5x14 Cap Screw:4',
'M5x14 Cap Screw:4','M5x14 Cap Screw:4',#16608,#16632,
'M5x14 Cap Screw:4');
#336=NEXT_ASSEMBLY_USAGE_OCCURRENCE('M5x14 Cap Screw:5',
'M5x14 Cap Screw:5','M5x14 Cap Screw:5',#16608,#16632,
'M5x14 Cap Screw:5');
#337=NEXT_ASSEMBLY_USAGE_OCCURRENCE('M4x10 Cap Screw:2',
'M4x10 Cap Screw:2','M4x10 Cap Screw:2',#16608,#16633,
'M4x10 Cap Screw:2');
#338=NEXT_ASSEMBLY_USAGE_OCCURRENCE('Roller bracket (1):1',
'Roller bracket (1):1','Roller bracket (1):1',#16614,#16615,
'Roller bracket (1):1');
#339=NEXT_ASSEMBLY_USAGE_OCCURRENCE('Roller axle (1):1',
'Roller axle (1):1','Roller axle (1):1',#16614,#16616,
'Roller axle (1):1');
#340=NEXT_ASSEMBLY_USAGE_OCCURRENCE('Inner race spacer (2):1',
'Inner race spacer (2):1','Inner race spacer (2):1',#16614,#16617,
'Inner race spacer (2):1');
#341=NEXT_ASSEMBLY_USAGE_OCCURRENCE('Inner race spacer (3):1',
'Inner race spacer (3):1','Inner race spacer (3):1',#16614,#16618,
'Inner race spacer (3):1');
#342=NEXT_ASSEMBLY_USAGE_OCCURRENCE('Axle keeper (1):1',
'Axle keeper (1):1','Axle keeper (1):1',#16614,#16619,
'Axle keeper (1):1');
#343=NEXT_ASSEMBLY_USAGE_OCCURRENCE('M5x14 Cap Screw:6',
'M5x14 Cap Screw:6','M5x14 Cap Screw:6',#16614,#16632,
'M5x14 Cap Screw:6');
#344=NEXT_ASSEMBLY_USAGE_OCCURRENCE('M5x14 Cap Screw:7',
'M5x14 Cap Screw:7','M5x14 Cap Screw:7',#16614,#16632,
'M5x14 Cap Screw:7');
#345=NEXT_ASSEMBLY_USAGE_OCCURRENCE('M5x14 Cap Screw:8',
'M5x14 Cap Screw:8','M5x14 Cap Screw:8',#16614,#16632,
'M5x14 Cap Screw:8');
#346=NEXT_ASSEMBLY_USAGE_OCCURRENCE('M5x14 Cap Screw:9',
'M5x14 Cap Screw:9','M5x14 Cap Screw:9',#16614,#16632,
'M5x14 Cap Screw:9');
#347=NEXT_ASSEMBLY_USAGE_OCCURRENCE('M4x10 Cap Screw:3',
'M4x10 Cap Screw:3','M4x10 Cap Screw:3',#16614,#16633,
'M4x10 Cap Screw:3');
#348=NEXT_ASSEMBLY_USAGE_OCCURRENCE('Roller bracket (2):1',
'Roller bracket (2):1','Roller bracket (2):1',#16620,#16621,
'Roller bracket (2):1');
#349=NEXT_ASSEMBLY_USAGE_OCCURRENCE('Roller axle (2):1',
'Roller axle (2):1','Roller axle (2):1',#16620,#16622,
'Roller axle (2):1');
#350=NEXT_ASSEMBLY_USAGE_OCCURRENCE('Inner race spacer (4):1',
'Inner race spacer (4):1','Inner race spacer (4):1',#16620,#16623,
'Inner race spacer (4):1');
#351=NEXT_ASSEMBLY_USAGE_OCCURRENCE('Inner race spacer (5):1',
'Inner race spacer (5):1','Inner race spacer (5):1',#16620,#16624,
'Inner race spacer (5):1');
#352=NEXT_ASSEMBLY_USAGE_OCCURRENCE('Axle keeper (2):1',
'Axle keeper (2):1','Axle keeper (2):1',#16620,#16625,
'Axle keeper (2):1');
#353=NEXT_ASSEMBLY_USAGE_OCCURRENCE('M5x14 Cap Screw:10',
'M5x14 Cap Screw:10','M5x14 Cap Screw:10',#16620,#16632,
'M5x14 Cap Screw:10');
#354=NEXT_ASSEMBLY_USAGE_OCCURRENCE('M5x14 Cap Screw:11',
'M5x14 Cap Screw:11','M5x14 Cap Screw:11',#16620,#16632,
'M5x14 Cap Screw:11');
#355=NEXT_ASSEMBLY_USAGE_OCCURRENCE('M5x14 Cap Screw:12',
'M5x14 Cap Screw:12','M5x14 Cap Screw:12',#16620,#16632,
'M5x14 Cap Screw:12');
#356=NEXT_ASSEMBLY_USAGE_OCCURRENCE('M5x14 Cap Screw:13',
'M5x14 Cap Screw:13','M5x14 Cap Screw:13',#16620,#16632,
'M5x14 Cap Screw:13');
#357=NEXT_ASSEMBLY_USAGE_OCCURRENCE('M4x10 Cap Screw:4',
'M4x10 Cap Screw:4','M4x10 Cap Screw:4',#16620,#16633,
'M4x10 Cap Screw:4');
#358=NEXT_ASSEMBLY_USAGE_OCCURRENCE('Roller bracket (3):1',
'Roller bracket (3):1','Roller bracket (3):1',#16626,#16627,
'Roller bracket (3):1');
#359=NEXT_ASSEMBLY_USAGE_OCCURRENCE('Roller axle (3):1',
'Roller axle (3):1','Roller axle (3):1',#16626,#16628,
'Roller axle (3):1');
#360=NEXT_ASSEMBLY_USAGE_OCCURRENCE('Inner race spacer (6):1',
'Inner race spacer (6):1','Inner race spacer (6):1',#16626,#16629,
'Inner race spacer (6):1');
#361=NEXT_ASSEMBLY_USAGE_OCCURRENCE('Inner race spacer (7):1',
'Inner race spacer (7):1','Inner race spacer (7):1',#16626,#16630,
'Inner race spacer (7):1');
#362=NEXT_ASSEMBLY_USAGE_OCCURRENCE('Axle keeper (3):1',
'Axle keeper (3):1','Axle keeper (3):1',#16626,#16631,
'Axle keeper (3):1');
#363=NEXT_ASSEMBLY_USAGE_OCCURRENCE('M5x14 Cap Screw:14',
'M5x14 Cap Screw:14','M5x14 Cap Screw:14',#16626,#16632,
'M5x14 Cap Screw:14');
#364=NEXT_ASSEMBLY_USAGE_OCCURRENCE('M5x14 Cap Screw:15',
'M5x14 Cap Screw:15','M5x14 Cap Screw:15',#16626,#16632,
'M5x14 Cap Screw:15');
#365=NEXT_ASSEMBLY_USAGE_OCCURRENCE('M5x14 Cap Screw:16',
'M5x14 Cap Screw:16','M5x14 Cap Screw:16',#16626,#16632,
'M5x14 Cap Screw:16');
#366=NEXT_ASSEMBLY_USAGE_OCCURRENCE('M5x14 Cap Screw:17',
'M5x14 Cap Screw:17','M5x14 Cap Screw:17',#16626,#16632,
'M5x14 Cap Screw:17');
#367=NEXT_ASSEMBLY_USAGE_OCCURRENCE('M4x10 Cap Screw:5',
'M4x10 Cap Screw:5','M4x10 Cap Screw:5',#16626,#16633,
'M4x10 Cap Screw:5');
#368=NEXT_ASSEMBLY_USAGE_OCCURRENCE('Inner ring (1):1',
'Inner ring (1):1','Inner ring (1):1',#16650,#16651,'Inner ring (1):1');
#369=NEXT_ASSEMBLY_USAGE_OCCURRENCE('Outer ring (1):1',
'Outer ring (1):1','Outer ring (1):1',#16650,#16652,'Outer ring (1):1');
#370=NEXT_ASSEMBLY_USAGE_OCCURRENCE('Balls (1):1','Balls (1):1',
'Balls (1):1',#16650,#16653,'Balls (1):1');
#371=NEXT_ASSEMBLY_USAGE_OCCURRENCE('Cage (1):1','Cage (1):1',
'Cage (1):1',#16650,#16654,'Cage (1):1');
#372=NEXT_ASSEMBLY_USAGE_OCCURRENCE('Seals 2RS (1):1','Seals 2RS (1):1',
'Seals 2RS (1):1',#16650,#16655,'Seals 2RS (1):1');
#373=NEXT_ASSEMBLY_USAGE_OCCURRENCE('Roller tread:1','Roller tread:1',
'Roller tread:1',#16634,#16635,'Roller tread:1');
#374=NEXT_ASSEMBLY_USAGE_OCCURRENCE('Outer race retainer:1',
'Outer race retainer:1','Outer race retainer:1',#16634,#16636,
'Outer race retainer:1');
#375=NEXT_ASSEMBLY_USAGE_OCCURRENCE('Outer race retainer (1):1',
'Outer race retainer (1):1','Outer race retainer (1):1',#16634,#16637,
'Outer race retainer (1):1');
#376=NEXT_ASSEMBLY_USAGE_OCCURRENCE(
'Sealed Ball Bearing - 10 x 30 x 9 mm:2',
'Sealed Ball Bearing - 10 x 30 x 9 mm:2',
'Sealed Ball Bearing - 10 x 30 x 9 mm:2',#16634,#16650,
'Sealed Ball Bearing - 10 x 30 x 9 mm:2');
#377=NEXT_ASSEMBLY_USAGE_OCCURRENCE('Roller tread (1):1',
'Roller tread (1):1','Roller tread (1):1',#16638,#16639,
'Roller tread (1):1');
#378=NEXT_ASSEMBLY_USAGE_OCCURRENCE('Outer race retainer (2):1',
'Outer race retainer (2):1','Outer race retainer (2):1',#16638,#16640,
'Outer race retainer (2):1');
#379=NEXT_ASSEMBLY_USAGE_OCCURRENCE('Outer race retainer (3):1',
'Outer race retainer (3):1','Outer race retainer (3):1',#16638,#16641,
'Outer race retainer (3):1');
#380=NEXT_ASSEMBLY_USAGE_OCCURRENCE(
'Sealed Ball Bearing - 10 x 30 x 9 mm:3',
'Sealed Ball Bearing - 10 x 30 x 9 mm:3',
'Sealed Ball Bearing - 10 x 30 x 9 mm:3',#16638,#16650,
'Sealed Ball Bearing - 10 x 30 x 9 mm:3');
#381=NEXT_ASSEMBLY_USAGE_OCCURRENCE('Roller tread (2):1',
'Roller tread (2):1','Roller tread (2):1',#16642,#16643,
'Roller tread (2):1');
#382=NEXT_ASSEMBLY_USAGE_OCCURRENCE('Outer race retainer (4):1',
'Outer race retainer (4):1','Outer race retainer (4):1',#16642,#16644,
'Outer race retainer (4):1');
#383=NEXT_ASSEMBLY_USAGE_OCCURRENCE('Outer race retainer (5):1',
'Outer race retainer (5):1','Outer race retainer (5):1',#16642,#16645,
'Outer race retainer (5):1');
#384=NEXT_ASSEMBLY_USAGE_OCCURRENCE(
'Sealed Ball Bearing - 10 x 30 x 9 mm:4',
'Sealed Ball Bearing - 10 x 30 x 9 mm:4',
'Sealed Ball Bearing - 10 x 30 x 9 mm:4',#16642,#16650,
'Sealed Ball Bearing - 10 x 30 x 9 mm:4');
#385=NEXT_ASSEMBLY_USAGE_OCCURRENCE('Roller tread (3):1',
'Roller tread (3):1','Roller tread (3):1',#16646,#16647,
'Roller tread (3):1');
#386=NEXT_ASSEMBLY_USAGE_OCCURRENCE('Outer race retainer (6):1',
'Outer race retainer (6):1','Outer race retainer (6):1',#16646,#16648,
'Outer race retainer (6):1');
#387=NEXT_ASSEMBLY_USAGE_OCCURRENCE('Outer race retainer (7):1',
'Outer race retainer (7):1','Outer race retainer (7):1',#16646,#16649,
'Outer race retainer (7):1');
#388=NEXT_ASSEMBLY_USAGE_OCCURRENCE(
'Sealed Ball Bearing - 10 x 30 x 9 mm:5',
'Sealed Ball Bearing - 10 x 30 x 9 mm:5',
'Sealed Ball Bearing - 10 x 30 x 9 mm:5',#16646,#16650,
'Sealed Ball Bearing - 10 x 30 x 9 mm:5');
#389=NEXT_ASSEMBLY_USAGE_OCCURRENCE('Base and centre bearing:1',
'Base and centre bearing:1','Base and centre bearing:1',#16588,#16589,
'Base and centre bearing:1');
#390=NEXT_ASSEMBLY_USAGE_OCCURRENCE('Turntable:1','Turntable:1',
'Turntable:1',#16588,#16602,'Turntable:1');
#391=NEXT_ASSEMBLY_USAGE_OCCURRENCE('Mount 1:1','Mount 1:1','Mount 1:1',
#16588,#16608,'Mount 1:1');
#392=NEXT_ASSEMBLY_USAGE_OCCURRENCE('Mount 2:1','Mount 2:1','Mount 2:1',
#16588,#16614,'Mount 2:1');
#393=NEXT_ASSEMBLY_USAGE_OCCURRENCE('Mount 3:1','Mount 3:1','Mount 3:1',
#16588,#16620,'Mount 3:1');
#394=NEXT_ASSEMBLY_USAGE_OCCURRENCE('Mount 4:1','Mount 4:1','Mount 4:1',
#16588,#16626,'Mount 4:1');
#395=NEXT_ASSEMBLY_USAGE_OCCURRENCE('Roller 1:1','Roller 1:1',
'Roller 1:1',#16588,#16634,'Roller 1:1');
#396=NEXT_ASSEMBLY_USAGE_OCCURRENCE('Roller 2:1','Roller 2:1',
'Roller 2:1',#16588,#16638,'Roller 2:1');
#397=NEXT_ASSEMBLY_USAGE_OCCURRENCE('Roller 3:1','Roller 3:1',
'Roller 3:1',#16588,#16642,'Roller 3:1');
#398=NEXT_ASSEMBLY_USAGE_OCCURRENCE('Roller 4:1','Roller 4:1',
'Roller 4:1',#16588,#16646,'Roller 4:1');
#399=B_SPLINE_CURVE_WITH_KNOTS('',3,(#13508,#13509,#13510,#13511,#13512,
#13513,#13514,#13515,#13516,#13517,#13518,#13519,#13520,#13521,#13522,#13523,
#13524,#13525,#13526,#13527,#13528,#13529),.UNSPECIFIED.,.F.,.F.,(4,2,2,
2,2,2,2,2,2,2,4),(0.0789043916784349,0.21052649634152,0.31578974451228,
0.421052992683041,0.522171766675512,0.623290540667983,0.724409314660453,
0.825528088652924,0.930791336823684,1.03605458499444,1.16767668965753),
 .UNSPECIFIED.);
#400=B_SPLINE_CURVE_WITH_KNOTS('',3,(#13533,#13534,#13535,#13536,#13537,
#13538,#13539,#13540,#13541,#13542,#13543,#13544,#13545,#13546,#13547,#13548,
#13549,#13550,#13551,#13552,#13553,#13554),.UNSPECIFIED.,.F.,.F.,(4,2,2,
2,2,2,2,2,2,2,4),(0.0774711646211702,0.142095081356994,0.284190162713987,
0.410912155766437,0.514012992401139,0.617113829035841,0.720214665670543,
0.823315502305246,0.950037495357694,1.09213257671469,1.15675649345051),
 .UNSPECIFIED.);
#401=B_SPLINE_CURVE_WITH_KNOTS('',3,(#13560,#13561,#13562,#13563,#13564,
#13565,#13566,#13567,#13568,#13569,#13570,#13571,#13572,#13573,#13574,#13575,
#13576,#13577,#13578,#13579,#13580,#13581),.UNSPECIFIED.,.F.,.F.,(4,2,2,
2,2,2,2,2,2,2,4),(0.0774711646211703,0.142095081356994,0.284190162713988,
0.410912155766436,0.514012992401139,0.617113829035841,0.720214665670544,
0.823315502305246,0.950037495357695,1.09213257671469,1.15675649345051),
 .UNSPECIFIED.);
#402=B_SPLINE_CURVE_WITH_KNOTS('',3,(#13585,#13586,#13587,#13588,#13589,
#13590,#13591,#13592,#13593,#13594,#13595,#13596,#13597,#13598,#13599,#13600,
#13601,#13602,#13603,#13604,#13605,#13606),.UNSPECIFIED.,.F.,.F.,(4,2,2,
2,2,2,2,2,2,2,4),(0.0774711646211702,0.142095081356994,0.284190162713988,
0.410912155766436,0.514012992401139,0.617113829035841,0.720214665670544,
0.823315502305246,0.950037495357695,1.09213257671469,1.15675649345051),
 .UNSPECIFIED.);
#403=B_SPLINE_CURVE_WITH_KNOTS('',3,(#13610,#13611,#13612,#13613,#13614,
#13615,#13616,#13617,#13618,#13619,#13620,#13621,#13622,#13623,#13624,#13625,
#13626,#13627,#13628,#13629,#13630,#13631),.UNSPECIFIED.,.F.,.F.,(4,2,2,
2,2,2,2,2,2,2,4),(0.0774711646211702,0.142095081356994,0.284190162713988,
0.410912155766436,0.514012992401139,0.617113829035842,0.720214665670544,
0.823315502305246,0.950037495357696,1.09213257671469,1.15675649345051),
 .UNSPECIFIED.);
#404=B_SPLINE_CURVE_WITH_KNOTS('',3,(#13640,#13641,#13642,#13643,#13644,
#13645,#13646,#13647,#13648,#13649,#13650,#13651,#13652,#13653,#13654,#13655,
#13656,#13657,#13658,#13659,#13660,#13661),.UNSPECIFIED.,.F.,.F.,(4,2,2,
2,2,2,2,2,2,2,4),(0.0774711646211702,0.142095081356994,0.284190162713987,
0.410912155766436,0.514012992401139,0.617113829035841,0.720214665670543,
0.823315502305246,0.950037495357695,1.09213257671469,1.15675649345051),
 .UNSPECIFIED.);
#405=B_SPLINE_CURVE_WITH_KNOTS('',3,(#13665,#13666,#13667,#13668,#13669,
#13670,#13671,#13672,#13673,#13674,#13675,#13676,#13677,#13678,#13679,#13680,
#13681,#13682,#13683,#13684,#13685,#13686),.UNSPECIFIED.,.F.,.F.,(4,2,2,
2,2,2,2,2,2,2,4),(0.0774711646211702,0.142095081356994,0.284190162713987,
0.410912155766436,0.514012992401139,0.617113829035841,0.720214665670543,
0.823315502305246,0.950037495357695,1.09213257671469,1.15675649345051),
 .UNSPECIFIED.);
#406=B_SPLINE_CURVE_WITH_KNOTS('',3,(#13690,#13691,#13692,#13693,#13694,
#13695,#13696,#13697,#13698,#13699,#13700,#13701,#13702,#13703,#13704,#13705,
#13706,#13707,#13708,#13709,#13710,#13711),.UNSPECIFIED.,.F.,.F.,(4,2,2,
2,2,2,2,2,2,2,4),(0.0774711646211703,0.142095081356994,0.284190162713988,
0.410912155766437,0.514012992401139,0.617113829035841,0.720214665670544,
0.823315502305247,0.950037495357696,1.09213257671469,1.15675649345051),
 .UNSPECIFIED.);
#407=B_SPLINE_CURVE_WITH_KNOTS('',3,(#13715,#13716,#13717,#13718,#13719,
#13720,#13721,#13722,#13723,#13724,#13725,#13726,#13727,#13728,#13729,#13730,
#13731,#13732,#13733,#13734,#13735,#13736),.UNSPECIFIED.,.F.,.F.,(4,2,2,
2,2,2,2,2,2,2,4),(0.0774711646211703,0.142095081356994,0.284190162713987,
0.410912155766436,0.514012992401139,0.617113829035841,0.720214665670543,
0.823315502305245,0.950037495357694,1.09213257671469,1.15675649345051),
 .UNSPECIFIED.);
#408=B_SPLINE_CURVE_WITH_KNOTS('',3,(#13740,#13741,#13742,#13743,#13744,
#13745,#13746,#13747,#13748,#13749,#13750,#13751,#13752,#13753,#13754,#13755,
#13756,#13757,#13758,#13759,#13760,#13761),.UNSPECIFIED.,.F.,.F.,(4,2,2,
2,2,2,2,2,2,2,4),(0.0774711646211703,0.142095081356994,0.284190162713988,
0.410912155766437,0.514012992401139,0.617113829035841,0.720214665670544,
0.823315502305246,0.950037495357695,1.09213257671469,1.15675649345051),
 .UNSPECIFIED.);
#409=B_SPLINE_CURVE_WITH_KNOTS('',3,(#13769,#13770,#13771,#13772,#13773,
#13774,#13775,#13776,#13777,#13778,#13779,#13780,#13781,#13782,#13783,#13784,
#13785,#13786,#13787,#13788,#13789,#13790),.UNSPECIFIED.,.F.,.F.,(4,2,2,
2,2,2,2,2,2,2,4),(0.0789043916784349,0.21052649634152,0.315789744512281,
0.421052992683041,0.522171766675512,0.623290540667983,0.724409314660453,
0.825528088652924,0.930791336823684,1.03605458499444,1.16767668965753),
 .UNSPECIFIED.);
#410=B_SPLINE_CURVE_WITH_KNOTS('',3,(#13798,#13799,#13800,#13801,#13802,
#13803,#13804,#13805,#13806,#13807,#13808,#13809,#13810,#13811,#13812,#13813,
#13814,#13815,#13816,#13817,#13818,#13819),.UNSPECIFIED.,.F.,.F.,(4,2,2,
2,2,2,2,2,2,2,4),(0.0789043916784348,0.210526496341521,0.315789744512281,
0.421052992683042,0.522171766675513,0.623290540667983,0.724409314660454,
0.825528088652925,0.930791336823685,1.03605458499444,1.16767668965753),
 .UNSPECIFIED.);
#411=B_SPLINE_CURVE_WITH_KNOTS('',3,(#13827,#13828,#13829,#13830,#13831,
#13832,#13833,#13834,#13835,#13836,#13837,#13838,#13839,#13840,#13841,#13842,
#13843,#13844,#13845,#13846,#13847,#13848),.UNSPECIFIED.,.F.,.F.,(4,2,2,
2,2,2,2,2,2,2,4),(0.0789043916784349,0.21052649634152,0.31578974451228,
0.421052992683041,0.522171766675511,0.623290540667982,0.724409314660453,
0.825528088652924,0.930791336823685,1.03605458499444,1.16767668965753),
 .UNSPECIFIED.);
#412=B_SPLINE_CURVE_WITH_KNOTS('',3,(#13858,#13859,#13860,#13861,#13862,
#13863,#13864,#13865,#13866,#13867,#13868,#13869,#13870,#13871,#13872,#13873,
#13874,#13875,#13876,#13877,#13878,#13879),.UNSPECIFIED.,.F.,.F.,(4,2,2,
2,2,2,2,2,2,2,4),(0.0789043916784348,0.21052649634152,0.315789744512281,
0.421052992683041,0.522171766675511,0.623290540667982,0.724409314660453,
0.825528088652924,0.930791336823684,1.03605458499444,1.16767668965753),
 .UNSPECIFIED.);
#413=B_SPLINE_CURVE_WITH_KNOTS('',3,(#13887,#13888,#13889,#13890,#13891,
#13892,#13893,#13894,#13895,#13896,#13897,#13898,#13899,#13900,#13901,#13902,
#13903,#13904,#13905,#13906,#13907,#13908),.UNSPECIFIED.,.F.,.F.,(4,2,2,
2,2,2,2,2,2,2,4),(0.0789043916784348,0.21052649634152,0.31578974451228,
0.42105299268304,0.522171766675511,0.623290540667982,0.724409314660453,
0.825528088652924,0.930791336823684,1.03605458499444,1.16767668965753),
 .UNSPECIFIED.);
#414=B_SPLINE_CURVE_WITH_KNOTS('',3,(#13916,#13917,#13918,#13919,#13920,
#13921,#13922,#13923,#13924,#13925,#13926,#13927,#13928,#13929,#13930,#13931,
#13932,#13933,#13934,#13935,#13936,#13937),.UNSPECIFIED.,.F.,.F.,(4,2,2,
2,2,2,2,2,2,2,4),(0.0789043916784348,0.21052649634152,0.315789744512281,
0.421052992683041,0.522171766675512,0.623290540667982,0.724409314660453,
0.825528088652924,0.930791336823684,1.03605458499444,1.16767668965753),
 .UNSPECIFIED.);
#415=B_SPLINE_CURVE_WITH_KNOTS('',3,(#13945,#13946,#13947,#13948,#13949,
#13950,#13951,#13952,#13953,#13954,#13955,#13956,#13957,#13958,#13959,#13960,
#13961,#13962,#13963,#13964,#13965,#13966),.UNSPECIFIED.,.F.,.F.,(4,2,2,
2,2,2,2,2,2,2,4),(0.0789043916784349,0.21052649634152,0.31578974451228,
0.42105299268304,0.522171766675511,0.623290540667982,0.724409314660453,
0.825528088652924,0.930791336823684,1.03605458499444,1.16767668965753),
 .UNSPECIFIED.);
#416=B_SPLINE_CURVE_WITH_KNOTS('',3,(#13975,#13976,#13977,#13978,#13979,
#13980,#13981,#13982,#13983,#13984,#13985,#13986,#13987,#13988,#13989,#13990,
#13991,#13992,#13993,#13994,#13995,#13996),.UNSPECIFIED.,.F.,.F.,(4,2,2,
2,2,2,2,2,2,2,4),(0.0789043916784348,0.21052649634152,0.31578974451228,
0.42105299268304,0.522171766675511,0.623290540667982,0.724409314660453,
0.825528088652924,0.930791336823684,1.03605458499444,1.16767668965753),
 .UNSPECIFIED.);
#417=B_SPLINE_CURVE_WITH_KNOTS('',3,(#14221,#14222,#14223,#14224,#14225,
#14226,#14227,#14228,#14229,#14230,#14231,#14232,#14233,#14234),
 .UNSPECIFIED.,.F.,.F.,(4,2,2,2,2,2,4),(0.714680326757343,0.792648662700719,
0.871912238073926,0.951175813447133,1.03043938882034,1.10970296419355,1.18767130013692),
 .UNSPECIFIED.);
#418=B_SPLINE_CURVE_WITH_KNOTS('',3,(#14237,#14238,#14239,#14240,#14241,
#14242,#14243,#14244,#14245,#14246,#14247,#14248,#14249,#14250),
 .UNSPECIFIED.,.F.,.F.,(4,2,2,2,2,2,4),(0.0805631177925872,0.158531453735963,
0.237795029109171,0.317058604482378,0.396322179855585,0.475585755228792,
0.553554091172168),.UNSPECIFIED.);
#419=B_SPLINE_CURVE_WITH_KNOTS('',3,(#14253,#14254,#14255,#14256,#14257,
#14258,#14259,#14260,#14261,#14262,#14263,#14264,#14265,#14266,#14267,#14268,
#14269,#14270,#14271,#14272,#14273,#14274,#14275,#14276,#14277,#14278,#14279,
#14280,#14281,#14282,#14283,#14284,#14285,#14286),.UNSPECIFIED.,.T.,.F.,
(4,2,2,2,2,2,2,2,2,2,2,2,2,2,2,2,4),(0.,0.0791819055472367,0.158363811094473,
0.237545215630595,0.316726620166717,0.395908024702839,0.475089429238961,
0.554271334786198,0.633453240333435,0.712635145880671,0.791817051427908,
0.87099845596403,0.950179860500152,1.02936126503627,1.1085426695724,1.18772457511963,
1.26690648066687),.UNSPECIFIED.);
#420=B_SPLINE_CURVE_WITH_KNOTS('',3,(#15640,#15641,#15642,#15643,#15644,
#15645,#15646,#15647,#15648,#15649,#15650,#15651,#15652,#15653,#15654,#15655,
#15656,#15657,#15658,#15659,#15660,#15661),.UNSPECIFIED.,.F.,.F.,(4,2,2,
2,2,2,2,2,2,2,4),(0.0473477652366656,0.126350602536658,0.189525903804987,
0.252701205073317,0.313298422430275,0.373895639787233,0.434492857144191,
0.495090074501149,0.558265375769478,0.621440677037807,0.7004435143378),
 .UNSPECIFIED.);
#421=B_SPLINE_CURVE_WITH_KNOTS('',3,(#15665,#15666,#15667,#15668,#15669,
#15670,#15671,#15672,#15673,#15674,#15675,#15676,#15677,#15678,#15679,#15680,
#15681,#15682,#15683,#15684,#15685,#15686),.UNSPECIFIED.,.F.,.F.,(4,2,2,
2,2,2,2,2,2,2,4),(0.0464897534940957,0.0852567806515119,0.170513561303024,
0.246687263103517,0.308657850341199,0.370628437578881,0.432599024816563,
0.494569612054245,0.570743313854739,0.656000094506251,0.694767121663666),
 .UNSPECIFIED.);
#422=B_SPLINE_CURVE_WITH_KNOTS('',3,(#15692,#15693,#15694,#15695,#15696,
#15697,#15698,#15699,#15700,#15701,#15702,#15703,#15704,#15705,#15706,#15707,
#15708,#15709,#15710,#15711,#15712,#15713),.UNSPECIFIED.,.F.,.F.,(4,2,2,
2,2,2,2,2,2,2,4),(0.0464897534940957,0.0852567806515118,0.170513561303024,
0.246687263103517,0.308657850341199,0.370628437578881,0.432599024816563,
0.494569612054245,0.570743313854738,0.65600009450625,0.694767121663666),
 .UNSPECIFIED.);
#423=B_SPLINE_CURVE_WITH_KNOTS('',3,(#15717,#15718,#15719,#15720,#15721,
#15722,#15723,#15724,#15725,#15726,#15727,#15728,#15729,#15730,#15731,#15732,
#15733,#15734,#15735,#15736,#15737,#15738),.UNSPECIFIED.,.F.,.F.,(4,2,2,
2,2,2,2,2,2,2,4),(0.0464897534940957,0.0852567806515119,0.170513561303024,
0.246687263103517,0.308657850341199,0.370628437578881,0.432599024816563,
0.494569612054245,0.570743313854739,0.656000094506251,0.694767121663666),
 .UNSPECIFIED.);
#424=B_SPLINE_CURVE_WITH_KNOTS('',3,(#15742,#15743,#15744,#15745,#15746,
#15747,#15748,#15749,#15750,#15751,#15752,#15753),.UNSPECIFIED.,.F.,.F.,
(4,2,2,2,2,4),(0.0464897534940957,0.0852567806515119,0.170513561303024,
0.246687263103517,0.308657850341199,0.370628437578881),.UNSPECIFIED.);
#425=B_SPLINE_CURVE_WITH_KNOTS('',3,(#15758,#15759,#15760,#15761,#15762,
#15763,#15764,#15765,#15766,#15767,#15768,#15769),.UNSPECIFIED.,.F.,.F.,
(4,2,2,2,2,4),(0.370628437578881,0.432599024816563,0.494569612054245,0.570743313854738,
0.65600009450625,0.694767121663666),.UNSPECIFIED.);
#426=B_SPLINE_CURVE_WITH_KNOTS('',3,(#15773,#15774,#15775,#15776,#15777,
#15778,#15779,#15780,#15781,#15782,#15783,#15784,#15785,#15786,#15787,#15788,
#15789,#15790,#15791,#15792,#15793,#15794),.UNSPECIFIED.,.F.,.F.,(4,2,2,
2,2,2,2,2,2,2,4),(0.0464897534940957,0.0852567806515121,0.170513561303024,
0.246687263103518,0.308657850341199,0.370628437578881,0.432599024816563,
0.494569612054245,0.570743313854738,0.65600009450625,0.694767121663666),
 .UNSPECIFIED.);
#427=B_SPLINE_CURVE_WITH_KNOTS('',3,(#15798,#15799,#15800,#15801,#15802,
#15803,#15804,#15805,#15806,#15807,#15808,#15809,#15810,#15811,#15812,#15813,
#15814,#15815,#15816,#15817,#15818,#15819),.UNSPECIFIED.,.F.,.F.,(4,2,2,
2,2,2,2,2,2,2,4),(0.0464897534940957,0.0852567806515119,0.170513561303024,
0.246687263103517,0.308657850341199,0.370628437578881,0.432599024816563,
0.494569612054245,0.570743313854738,0.65600009450625,0.694767121663667),
 .UNSPECIFIED.);
#428=B_SPLINE_CURVE_WITH_KNOTS('',3,(#15823,#15824,#15825,#15826,#15827,
#15828,#15829,#15830,#15831,#15832,#15833,#15834,#15835,#15836,#15837,#15838,
#15839,#15840,#15841,#15842,#15843,#15844),.UNSPECIFIED.,.F.,.F.,(4,2,2,
2,2,2,2,2,2,2,4),(0.0464897534940957,0.0852567806515119,0.170513561303024,
0.246687263103517,0.308657850341199,0.370628437578881,0.432599024816563,
0.494569612054245,0.570743313854738,0.65600009450625,0.694767121663666),
 .UNSPECIFIED.);
#429=B_SPLINE_CURVE_WITH_KNOTS('',3,(#15848,#15849,#15850,#15851,#15852,
#15853,#15854,#15855,#15856,#15857,#15858,#15859,#15860,#15861,#15862,#15863,
#15864,#15865,#15866,#15867,#15868,#15869),.UNSPECIFIED.,.F.,.F.,(4,2,2,
2,2,2,2,2,2,2,4),(0.0464897534940957,0.0852567806515119,0.170513561303024,
0.246687263103517,0.308657850341199,0.370628437578881,0.432599024816563,
0.494569612054245,0.570743313854739,0.656000094506251,0.694767121663667),
 .UNSPECIFIED.);
#430=B_SPLINE_CURVE_WITH_KNOTS('',3,(#15877,#15878,#15879,#15880,#15881,
#15882,#15883,#15884,#15885,#15886,#15887,#15888,#15889,#15890,#15891,#15892,
#15893,#15894,#15895,#15896,#15897,#15898),.UNSPECIFIED.,.F.,.F.,(4,2,2,
2,2,2,2,2,2,2,4),(0.0473477652366656,0.126350602536658,0.189525903804987,
0.252701205073316,0.313298422430274,0.373895639787232,0.434492857144191,
0.495090074501149,0.558265375769478,0.621440677037807,0.7004435143378),
 .UNSPECIFIED.);
#431=B_SPLINE_CURVE_WITH_KNOTS('',3,(#15906,#15907,#15908,#15909,#15910,
#15911,#15912,#15913,#15914,#15915,#15916,#15917,#15918,#15919,#15920,#15921,
#15922,#15923,#15924,#15925,#15926,#15927),.UNSPECIFIED.,.F.,.F.,(4,2,2,
2,2,2,2,2,2,2,4),(0.0473477652366656,0.126350602536658,0.189525903804987,
0.252701205073317,0.313298422430275,0.373895639787233,0.434492857144191,
0.495090074501149,0.558265375769478,0.621440677037807,0.7004435143378),
 .UNSPECIFIED.);
#432=B_SPLINE_CURVE_WITH_KNOTS('',3,(#15936,#15937,#15938,#15939,#15940,
#15941,#15942,#15943,#15944,#15945,#15946,#15947),.UNSPECIFIED.,.F.,.F.,
(4,2,2,2,2,4),(0.0473477652366656,0.126350602536658,0.189525903804987,0.252701205073316,
0.313298422430275,0.373895639787233),.UNSPECIFIED.);
#433=B_SPLINE_CURVE_WITH_KNOTS('',3,(#15949,#15950,#15951,#15952,#15953,
#15954,#15955,#15956,#15957,#15958,#15959,#15960),.UNSPECIFIED.,.F.,.F.,
(4,2,2,2,2,4),(0.373895639787233,0.434492857144191,0.495090074501149,0.558265375769478,
0.621440677037807,0.7004435143378),.UNSPECIFIED.);
#434=B_SPLINE_CURVE_WITH_KNOTS('',3,(#15967,#15968,#15969,#15970,#15971,
#15972,#15973,#15974,#15975,#15976,#15977,#15978,#15979,#15980,#15981,#15982,
#15983,#15984,#15985,#15986,#15987,#15988),.UNSPECIFIED.,.F.,.F.,(4,2,2,
2,2,2,2,2,2,2,4),(0.0473477652366656,0.126350602536658,0.189525903804987,
0.252701205073316,0.313298422430275,0.373895639787233,0.434492857144191,
0.495090074501149,0.558265375769478,0.621440677037807,0.7004435143378),
 .UNSPECIFIED.);
#435=B_SPLINE_CURVE_WITH_KNOTS('',3,(#15996,#15997,#15998,#15999,#16000,
#16001,#16002,#16003,#16004,#16005,#16006,#16007,#16008,#16009,#16010,#16011,
#16012,#16013,#16014,#16015,#16016,#16017),.UNSPECIFIED.,.F.,.F.,(4,2,2,
2,2,2,2,2,2,2,4),(0.0473477652366656,0.126350602536658,0.189525903804987,
0.252701205073317,0.313298422430275,0.373895639787233,0.434492857144191,
0.495090074501149,0.558265375769478,0.621440677037807,0.7004435143378),
 .UNSPECIFIED.);
#436=B_SPLINE_CURVE_WITH_KNOTS('',3,(#16025,#16026,#16027,#16028,#16029,
#16030,#16031,#16032,#16033,#16034,#16035,#16036,#16037,#16038,#16039,#16040,
#16041,#16042,#16043,#16044,#16045,#16046),.UNSPECIFIED.,.F.,.F.,(4,2,2,
2,2,2,2,2,2,2,4),(0.0473477652366656,0.126350602536658,0.189525903804987,
0.252701205073316,0.313298422430275,0.373895639787233,0.434492857144191,
0.495090074501149,0.558265375769478,0.621440677037807,0.7004435143378),
 .UNSPECIFIED.);
#437=B_SPLINE_CURVE_WITH_KNOTS('',3,(#16055,#16056,#16057,#16058,#16059,
#16060,#16061,#16062,#16063,#16064,#16065,#16066,#16067,#16068,#16069,#16070,
#16071,#16072,#16073,#16074,#16075,#16076),.UNSPECIFIED.,.F.,.F.,(4,2,2,
2,2,2,2,2,2,2,4),(0.0473477652366656,0.126350602536658,0.189525903804987,
0.252701205073317,0.313298422430275,0.373895639787233,0.434492857144191,
0.495090074501149,0.558265375769478,0.621440677037807,0.7004435143378),
 .UNSPECIFIED.);
#438=SPHERICAL_SURFACE('',#9272,0.3969);
#439=SPHERICAL_SURFACE('',#9274,0.3969);
#440=SPHERICAL_SURFACE('',#9276,0.3969);
#441=SPHERICAL_SURFACE('',#9278,0.3969);
#442=SPHERICAL_SURFACE('',#9280,0.3969);
#443=SPHERICAL_SURFACE('',#9282,0.3969);
#444=SPHERICAL_SURFACE('',#9284,0.3969);
#445=SPHERICAL_SURFACE('',#9286,0.3969);
#446=SPHERICAL_SURFACE('',#9288,0.3969);
#447=SPHERICAL_SURFACE('',#9291,0.412776);
#448=SPHERICAL_SURFACE('',#9309,0.412776);
#449=SPHERICAL_SURFACE('',#9314,0.412776);
#450=SPHERICAL_SURFACE('',#9319,0.412776);
#451=SPHERICAL_SURFACE('',#9325,0.412776);
#452=SPHERICAL_SURFACE('',#9330,0.412776);
#453=SPHERICAL_SURFACE('',#9335,0.412776);
#454=SPHERICAL_SURFACE('',#9340,0.412776);
#455=SPHERICAL_SURFACE('',#9348,0.412776);
#456=SPHERICAL_SURFACE('',#10082,0.23815);
#457=SPHERICAL_SURFACE('',#10084,0.23815);
#458=SPHERICAL_SURFACE('',#10086,0.23815);
#459=SPHERICAL_SURFACE('',#10088,0.23815);
#460=SPHERICAL_SURFACE('',#10090,0.23815);
#461=SPHERICAL_SURFACE('',#10092,0.23815);
#462=SPHERICAL_SURFACE('',#10094,0.23815);
#463=SPHERICAL_SURFACE('',#10096,0.23815);
#464=SPHERICAL_SURFACE('',#10099,0.247676);
#465=SPHERICAL_SURFACE('',#10115,0.247676);
#466=SPHERICAL_SURFACE('',#10120,0.247676);
#467=SPHERICAL_SURFACE('',#10125,0.247676);
#468=SPHERICAL_SURFACE('',#10130,0.247676);
#469=SPHERICAL_SURFACE('',#10135,0.247676);
#470=SPHERICAL_SURFACE('',#10140,0.247676);
#471=SPHERICAL_SURFACE('',#10148,0.247676);
#472=TOROIDAL_SURFACE('',#9232,1.925,0.412776);
#473=TOROIDAL_SURFACE('',#9252,1.925,0.412776);
#474=TOROIDAL_SURFACE('',#10042,1.,0.247676);
#475=TOROIDAL_SURFACE('',#10062,1.,0.247676);
#476=CONICAL_SURFACE('',#9219,0.475,0.785398163397449);
#477=CONICAL_SURFACE('',#9223,0.485,0.785398163397448);
#478=CONICAL_SURFACE('',#9227,0.31,0.463647609000806);
#479=CONICAL_SURFACE('',#9243,1.3,0.785398163397449);
#480=CONICAL_SURFACE('',#9250,1.3,0.785398163397449);
#481=CONICAL_SURFACE('',#9263,2.55,0.785398163397449);
#482=CONICAL_SURFACE('',#9267,2.55,0.785398163397449);
#483=CONICAL_SURFACE('',#9471,0.325,0.785398163397448);
#484=CONICAL_SURFACE('',#9475,0.335,0.785398163397448);
#485=CONICAL_SURFACE('',#9479,0.21,0.463647609000806);
#486=CONICAL_SURFACE('',#9483,0.18,0.785398163397448);
#487=CONICAL_SURFACE('',#9518,0.235,0.785398163397448);
#488=CONICAL_SURFACE('',#9522,0.2125,0.785398163397448);
#489=CONICAL_SURFACE('',#9853,0.4,0.785398163397448);
#490=CONICAL_SURFACE('',#9857,0.41,0.785398163397448);
#491=CONICAL_SURFACE('',#9861,0.26,0.463647609000806);
#492=CONICAL_SURFACE('',#9877,0.325,0.785398163397448);
#493=CONICAL_SURFACE('',#9881,0.335,0.785398163397448);
#494=CONICAL_SURFACE('',#9885,0.21,0.463647609000806);
#495=CONICAL_SURFACE('',#10053,0.53,0.785398163397448);
#496=CONICAL_SURFACE('',#10060,0.53,0.785398163397448);
#497=CONICAL_SURFACE('',#10073,1.47,0.785398163397449);
#498=CONICAL_SURFACE('',#10077,1.47,0.785398163397449);
#499=ORIENTED_CLOSED_SHELL('',*,#8361,.F.);
#500=ORIENTED_CLOSED_SHELL('',*,#8383,.F.);
#501=ORIENTED_CLOSED_SHELL('',*,#8405,.F.);
#502=ORIENTED_CLOSED_SHELL('',*,#8407,.F.);
#503=BREP_WITH_VOIDS('Body1',#8362,(#499));
#504=BREP_WITH_VOIDS('Body1',#8382,(#500));
#505=BREP_WITH_VOIDS('Body1',#8406,(#501));
#506=BREP_WITH_VOIDS('Body1',#8408,(#502));
#507=SHAPE_REPRESENTATION_RELATIONSHIP('SRR','None',#16521,#562);
#508=SHAPE_REPRESENTATION_RELATIONSHIP('SRR','None',#16522,#563);
#509=SHAPE_REPRESENTATION_RELATIONSHIP('SRR','None',#16523,#564);
#510=SHAPE_REPRESENTATION_RELATIONSHIP('SRR','None',#16524,#565);
#511=SHAPE_REPRESENTATION_RELATIONSHIP('SRR','None',#16526,#566);
#512=SHAPE_REPRESENTATION_RELATIONSHIP('SRR','None',#16527,#567);
#513=SHAPE_REPRESENTATION_RELATIONSHIP('SRR','None',#16528,#568);
#514=SHAPE_REPRESENTATION_RELATIONSHIP('SRR','None',#16529,#569);
#515=SHAPE_REPRESENTATION_RELATIONSHIP('SRR','None',#16530,#570);
#516=SHAPE_REPRESENTATION_RELATIONSHIP('SRR','None',#16531,#571);
#517=SHAPE_REPRESENTATION_RELATIONSHIP('SRR','None',#16532,#572);
#518=SHAPE_REPRESENTATION_RELATIONSHIP('SRR','None',#16534,#573);
#519=SHAPE_REPRESENTATION_RELATIONSHIP('SRR','None',#16535,#574);
#520=SHAPE_REPRESENTATION_RELATIONSHIP('SRR','None',#16536,#575);
#521=SHAPE_REPRESENTATION_RELATIONSHIP('SRR','None',#16537,#576);
#522=SHAPE_REPRESENTATION_RELATIONSHIP('SRR','None',#16538,#577);
#523=SHAPE_REPRESENTATION_RELATIONSHIP('SRR','None',#16540,#578);
#524=SHAPE_REPRESENTATION_RELATIONSHIP('SRR','None',#16541,#579);
#525=SHAPE_REPRESENTATION_RELATIONSHIP('SRR','None',#16542,#580);
#526=SHAPE_REPRESENTATION_RELATIONSHIP('SRR','None',#16543,#581);
#527=SHAPE_REPRESENTATION_RELATIONSHIP('SRR','None',#16544,#582);
#528=SHAPE_REPRESENTATION_RELATIONSHIP('SRR','None',#16546,#583);
#529=SHAPE_REPRESENTATION_RELATIONSHIP('SRR','None',#16547,#584);
#530=SHAPE_REPRESENTATION_RELATIONSHIP('SRR','None',#16548,#585);
#531=SHAPE_REPRESENTATION_RELATIONSHIP('SRR','None',#16549,#586);
#532=SHAPE_REPRESENTATION_RELATIONSHIP('SRR','None',#16550,#587);
#533=SHAPE_REPRESENTATION_RELATIONSHIP('SRR','None',#16552,#588);
#534=SHAPE_REPRESENTATION_RELATIONSHIP('SRR','None',#16553,#589);
#535=SHAPE_REPRESENTATION_RELATIONSHIP('SRR','None',#16554,#590);
#536=SHAPE_REPRESENTATION_RELATIONSHIP('SRR','None',#16555,#591);
#537=SHAPE_REPRESENTATION_RELATIONSHIP('SRR','None',#16556,#592);
#538=SHAPE_REPRESENTATION_RELATIONSHIP('SRR','None',#16558,#593);
#539=SHAPE_REPRESENTATION_RELATIONSHIP('SRR','None',#16559,#594);
#540=SHAPE_REPRESENTATION_RELATIONSHIP('SRR','None',#16560,#595);
#541=SHAPE_REPRESENTATION_RELATIONSHIP('SRR','None',#16561,#596);
#542=SHAPE_REPRESENTATION_RELATIONSHIP('SRR','None',#16562,#597);
#543=SHAPE_REPRESENTATION_RELATIONSHIP('SRR','None',#16563,#598);
#544=SHAPE_REPRESENTATION_RELATIONSHIP('SRR','None',#16564,#599);
#545=SHAPE_REPRESENTATION_RELATIONSHIP('SRR','None',#16566,#600);
#546=SHAPE_REPRESENTATION_RELATIONSHIP('SRR','None',#16567,#601);
#547=SHAPE_REPRESENTATION_RELATIONSHIP('SRR','None',#16568,#602);
#548=SHAPE_REPRESENTATION_RELATIONSHIP('SRR','None',#16570,#603);
#549=SHAPE_REPRESENTATION_RELATIONSHIP('SRR','None',#16571,#604);
#550=SHAPE_REPRESENTATION_RELATIONSHIP('SRR','None',#16572,#605);
#551=SHAPE_REPRESENTATION_RELATIONSHIP('SRR','None',#16574,#606);
#552=SHAPE_REPRESENTATION_RELATIONSHIP('SRR','None',#16575,#607);
#553=SHAPE_REPRESENTATION_RELATIONSHIP('SRR','None',#16576,#608);
#554=SHAPE_REPRESENTATION_RELATIONSHIP('SRR','None',#16578,#609);
#555=SHAPE_REPRESENTATION_RELATIONSHIP('SRR','None',#16579,#610);
#556=SHAPE_REPRESENTATION_RELATIONSHIP('SRR','None',#16580,#611);
#557=SHAPE_REPRESENTATION_RELATIONSHIP('SRR','None',#16582,#612);
#558=SHAPE_REPRESENTATION_RELATIONSHIP('SRR','None',#16583,#613);
#559=SHAPE_REPRESENTATION_RELATIONSHIP('SRR','None',#16584,#614);
#560=SHAPE_REPRESENTATION_RELATIONSHIP('SRR','None',#16585,#615);
#561=SHAPE_REPRESENTATION_RELATIONSHIP('SRR','None',#16586,#616);
#562=ADVANCED_BREP_SHAPE_REPRESENTATION('',(#689),#16215);
#563=ADVANCED_BREP_SHAPE_REPRESENTATION('',(#690),#16216);
#564=ADVANCED_BREP_SHAPE_REPRESENTATION('',(#691),#16217);
#565=ADVANCED_BREP_SHAPE_REPRESENTATION('',(#503),#16218);
#566=ADVANCED_BREP_SHAPE_REPRESENTATION('',(#692),#16220);
#567=ADVANCED_BREP_SHAPE_REPRESENTATION('',(#693),#16221);
#568=ADVANCED_BREP_SHAPE_REPRESENTATION('',(#694,#695,#696,#697,#698,#699,
#700,#701,#702),#16222);
#569=ADVANCED_BREP_SHAPE_REPRESENTATION('',(#703),#16223);
#570=ADVANCED_BREP_SHAPE_REPRESENTATION('',(#704,#705),#16224);
#571=ADVANCED_BREP_SHAPE_REPRESENTATION('',(#706),#16225);
#572=ADVANCED_BREP_SHAPE_REPRESENTATION('',(#707),#16226);
#573=ADVANCED_BREP_SHAPE_REPRESENTATION('',(#708),#16228);
#574=ADVANCED_BREP_SHAPE_REPRESENTATION('',(#709),#16229);
#575=ADVANCED_BREP_SHAPE_REPRESENTATION('',(#710),#16230);
#576=ADVANCED_BREP_SHAPE_REPRESENTATION('',(#504),#16231);
#577=ADVANCED_BREP_SHAPE_REPRESENTATION('',(#711),#16232);
#578=ADVANCED_BREP_SHAPE_REPRESENTATION('',(#712),#16234);
#579=ADVANCED_BREP_SHAPE_REPRESENTATION('',(#713),#16235);
#580=ADVANCED_BREP_SHAPE_REPRESENTATION('',(#714),#16236);
#581=ADVANCED_BREP_SHAPE_REPRESENTATION('',(#715),#16237);
#582=ADVANCED_BREP_SHAPE_REPRESENTATION('',(#716),#16238);
#583=ADVANCED_BREP_SHAPE_REPRESENTATION('',(#717),#16240);
#584=ADVANCED_BREP_SHAPE_REPRESENTATION('',(#718),#16241);
#585=ADVANCED_BREP_SHAPE_REPRESENTATION('',(#719),#16242);
#586=ADVANCED_BREP_SHAPE_REPRESENTATION('',(#720),#16243);
#587=ADVANCED_BREP_SHAPE_REPRESENTATION('',(#721),#16244);
#588=ADVANCED_BREP_SHAPE_REPRESENTATION('',(#722),#16246);
#589=ADVANCED_BREP_SHAPE_REPRESENTATION('',(#723),#16247);
#590=ADVANCED_BREP_SHAPE_REPRESENTATION('',(#724),#16248);
#591=ADVANCED_BREP_SHAPE_REPRESENTATION('',(#725),#16249);
#592=ADVANCED_BREP_SHAPE_REPRESENTATION('',(#726),#16250);
#593=ADVANCED_BREP_SHAPE_REPRESENTATION('',(#727),#16252);
#594=ADVANCED_BREP_SHAPE_REPRESENTATION('',(#728),#16253);
#595=ADVANCED_BREP_SHAPE_REPRESENTATION('',(#729),#16254);
#596=ADVANCED_BREP_SHAPE_REPRESENTATION('',(#730),#16255);
#597=ADVANCED_BREP_SHAPE_REPRESENTATION('',(#731),#16256);
#598=ADVANCED_BREP_SHAPE_REPRESENTATION('',(#505),#16257);
#599=ADVANCED_BREP_SHAPE_REPRESENTATION('',(#506),#16258);
#600=ADVANCED_BREP_SHAPE_REPRESENTATION('',(#732),#16260);
#601=ADVANCED_BREP_SHAPE_REPRESENTATION('',(#733),#16261);
#602=ADVANCED_BREP_SHAPE_REPRESENTATION('',(#734),#16262);
#603=ADVANCED_BREP_SHAPE_REPRESENTATION('',(#735),#16264);
#604=ADVANCED_BREP_SHAPE_REPRESENTATION('',(#736),#16265);
#605=ADVANCED_BREP_SHAPE_REPRESENTATION('',(#737),#16266);
#606=ADVANCED_BREP_SHAPE_REPRESENTATION('',(#738),#16268);
#607=ADVANCED_BREP_SHAPE_REPRESENTATION('',(#739),#16269);
#608=ADVANCED_BREP_SHAPE_REPRESENTATION('',(#740),#16270);
#609=ADVANCED_BREP_SHAPE_REPRESENTATION('',(#741),#16272);
#610=ADVANCED_BREP_SHAPE_REPRESENTATION('',(#742),#16273);
#611=ADVANCED_BREP_SHAPE_REPRESENTATION('',(#743),#16274);
#612=ADVANCED_BREP_SHAPE_REPRESENTATION('',(#744),#16276);
#613=ADVANCED_BREP_SHAPE_REPRESENTATION('',(#745),#16277);
#614=ADVANCED_BREP_SHAPE_REPRESENTATION('',(#746,#747,#748,#749,#750,#751,
#752,#753),#16278);
#615=ADVANCED_BREP_SHAPE_REPRESENTATION('',(#754),#16279);
#616=ADVANCED_BREP_SHAPE_REPRESENTATION('',(#755,#756),#16280);
#617=STYLED_ITEM('',(#16911),#689);
#618=STYLED_ITEM('',(#16911),#690);
#619=STYLED_ITEM('',(#16932),#691);
#620=STYLED_ITEM('',(#16939),#503);
#621=STYLED_ITEM('',(#16932),#692);
#622=STYLED_ITEM('',(#16932),#693);
#623=STYLED_ITEM('',(#16932),#694);
#624=STYLED_ITEM('',(#16932),#695);
#625=STYLED_ITEM('',(#16932),#696);
#626=STYLED_ITEM('',(#16932),#697);
#627=STYLED_ITEM('',(#16932),#698);
#628=STYLED_ITEM('',(#16932),#699);
#629=STYLED_ITEM('',(#16932),#700);
#630=STYLED_ITEM('',(#16932),#701);
#631=STYLED_ITEM('',(#16932),#702);
#632=STYLED_ITEM('',(#16932),#703);
#633=STYLED_ITEM('',(#16932),#704);
#634=STYLED_ITEM('',(#16932),#705);
#635=STYLED_ITEM('',(#16946),#706);
#636=STYLED_ITEM('',(#16946),#707);
#637=STYLED_ITEM('',(#16946),#708);
#638=STYLED_ITEM('',(#16925),#709);
#639=STYLED_ITEM('',(#16925),#710);
#640=STYLED_ITEM('',(#16939),#504);
#641=STYLED_ITEM('',(#16939),#711);
#642=STYLED_ITEM('',(#16911),#712);
#643=STYLED_ITEM('',(#16932),#713);
#644=STYLED_ITEM('',(#16932),#714);
#645=STYLED_ITEM('',(#16932),#715);
#646=STYLED_ITEM('',(#16932),#716);
#647=STYLED_ITEM('',(#16911),#717);
#648=STYLED_ITEM('',(#16932),#718);
#649=STYLED_ITEM('',(#16932),#719);
#650=STYLED_ITEM('',(#16932),#720);
#651=STYLED_ITEM('',(#16932),#721);
#652=STYLED_ITEM('',(#16911),#722);
#653=STYLED_ITEM('',(#16932),#723);
#654=STYLED_ITEM('',(#16932),#724);
#655=STYLED_ITEM('',(#16932),#725);
#656=STYLED_ITEM('',(#16932),#726);
#657=STYLED_ITEM('',(#16911),#727);
#658=STYLED_ITEM('',(#16932),#728);
#659=STYLED_ITEM('',(#16932),#729);
#660=STYLED_ITEM('',(#16932),#730);
#661=STYLED_ITEM('',(#16932),#731);
#662=STYLED_ITEM('',(#16939),#505);
#663=STYLED_ITEM('',(#16939),#506);
#664=STYLED_ITEM('',(#16925),#732);
#665=STYLED_ITEM('',(#16932),#733);
#666=STYLED_ITEM('',(#16932),#734);
#667=STYLED_ITEM('',(#16925),#735);
#668=STYLED_ITEM('',(#16932),#736);
#669=STYLED_ITEM('',(#16932),#737);
#670=STYLED_ITEM('',(#16925),#738);
#671=STYLED_ITEM('',(#16932),#739);
#672=STYLED_ITEM('',(#16932),#740);
#673=STYLED_ITEM('',(#16925),#741);
#674=STYLED_ITEM('',(#16932),#742);
#675=STYLED_ITEM('',(#16932),#743);
#676=STYLED_ITEM('',(#16932),#744);
#677=STYLED_ITEM('',(#16932),#745);
#678=STYLED_ITEM('',(#16932),#746);
#679=STYLED_ITEM('',(#16932),#747);
#680=STYLED_ITEM('',(#16932),#748);
#681=STYLED_ITEM('',(#16932),#749);
#682=STYLED_ITEM('',(#16932),#750);
#683=STYLED_ITEM('',(#16932),#751);
#684=STYLED_ITEM('',(#16932),#752);
#685=STYLED_ITEM('',(#16932),#753);
#686=STYLED_ITEM('',(#16932),#754);
#687=STYLED_ITEM('',(#16932),#755);
#688=STYLED_ITEM('',(#16932),#756);
#689=MANIFOLD_SOLID_BREP('Body1',#8358);
#690=MANIFOLD_SOLID_BREP('Body1',#8359);
#691=MANIFOLD_SOLID_BREP('Body1',#8360);
#692=MANIFOLD_SOLID_BREP('Body1',#8363);
#693=MANIFOLD_SOLID_BREP('Body1',#8364);
#694=MANIFOLD_SOLID_BREP('Body1',#8365);
#695=MANIFOLD_SOLID_BREP('Body2',#8366);
#696=MANIFOLD_SOLID_BREP('Body3',#8367);
#697=MANIFOLD_SOLID_BREP('Body4',#8368);
#698=MANIFOLD_SOLID_BREP('Body5',#8369);
#699=MANIFOLD_SOLID_BREP('Body6',#8370);
#700=MANIFOLD_SOLID_BREP('Body7',#8371);
#701=MANIFOLD_SOLID_BREP('Body8',#8372);
#702=MANIFOLD_SOLID_BREP('Body9',#8373);
#703=MANIFOLD_SOLID_BREP('Continuous crown cage',#8374);
#704=MANIFOLD_SOLID_BREP('Body1',#8375);
#705=MANIFOLD_SOLID_BREP('Body2',#8376);
#706=MANIFOLD_SOLID_BREP('Body1',#8377);
#707=MANIFOLD_SOLID_BREP('Body1',#8378);
#708=MANIFOLD_SOLID_BREP('Body1',#8379);
#709=MANIFOLD_SOLID_BREP('Body1',#8380);
#710=MANIFOLD_SOLID_BREP('Body1',#8381);
#711=MANIFOLD_SOLID_BREP('Body1',#8384);
#712=MANIFOLD_SOLID_BREP('Body1',#8385);
#713=MANIFOLD_SOLID_BREP('Body1',#8386);
#714=MANIFOLD_SOLID_BREP('Body1',#8387);
#715=MANIFOLD_SOLID_BREP('Body1',#8388);
#716=MANIFOLD_SOLID_BREP('Body1',#8389);
#717=MANIFOLD_SOLID_BREP('Body1',#8390);
#718=MANIFOLD_SOLID_BREP('Body1',#8391);
#719=MANIFOLD_SOLID_BREP('Body1',#8392);
#720=MANIFOLD_SOLID_BREP('Body1',#8393);
#721=MANIFOLD_SOLID_BREP('Body1',#8394);
#722=MANIFOLD_SOLID_BREP('Body1',#8395);
#723=MANIFOLD_SOLID_BREP('Body1',#8396);
#724=MANIFOLD_SOLID_BREP('Body1',#8397);
#725=MANIFOLD_SOLID_BREP('Body1',#8398);
#726=MANIFOLD_SOLID_BREP('Body1',#8399);
#727=MANIFOLD_SOLID_BREP('Body1',#8400);
#728=MANIFOLD_SOLID_BREP('Body1',#8401);
#729=MANIFOLD_SOLID_BREP('Body1',#8402);
#730=MANIFOLD_SOLID_BREP('Body1',#8403);
#731=MANIFOLD_SOLID_BREP('Body1',#8404);
#732=MANIFOLD_SOLID_BREP('Body1',#8409);
#733=MANIFOLD_SOLID_BREP('Body1',#8410);
#734=MANIFOLD_SOLID_BREP('Body1',#8411);
#735=MANIFOLD_SOLID_BREP('Body1',#8412);
#736=MANIFOLD_SOLID_BREP('Body1',#8413);
#737=MANIFOLD_SOLID_BREP('Body1',#8414);
#738=MANIFOLD_SOLID_BREP('Body1',#8415);
#739=MANIFOLD_SOLID_BREP('Body1',#8416);
#740=MANIFOLD_SOLID_BREP('Body1',#8417);
#741=MANIFOLD_SOLID_BREP('Body1',#8418);
#742=MANIFOLD_SOLID_BREP('Body1',#8419);
#743=MANIFOLD_SOLID_BREP('Body1',#8420);
#744=MANIFOLD_SOLID_BREP('Body1',#8421);
#745=MANIFOLD_SOLID_BREP('Body1',#8422);
#746=MANIFOLD_SOLID_BREP('Body1',#8423);
#747=MANIFOLD_SOLID_BREP('Body2',#8424);
#748=MANIFOLD_SOLID_BREP('Body3',#8425);
#749=MANIFOLD_SOLID_BREP('Body4',#8426);
#750=MANIFOLD_SOLID_BREP('Body5',#8427);
#751=MANIFOLD_SOLID_BREP('Body6',#8428);
#752=MANIFOLD_SOLID_BREP('Body7',#8429);
#753=MANIFOLD_SOLID_BREP('Body8',#8430);
#754=MANIFOLD_SOLID_BREP('Continuous crown cage',#8431);
#755=MANIFOLD_SOLID_BREP('Body1',#8432);
#756=MANIFOLD_SOLID_BREP('Body2',#8433);
#757=FACE_BOUND('',#1780,.T.);
#758=FACE_BOUND('',#1781,.T.);
#759=FACE_BOUND('',#1782,.T.);
#760=FACE_BOUND('',#1783,.T.);
#761=FACE_BOUND('',#1784,.T.);
#762=FACE_BOUND('',#1785,.T.);
#763=FACE_BOUND('',#1786,.T.);
#764=FACE_BOUND('',#1787,.T.);
#765=FACE_BOUND('',#1788,.T.);
#766=FACE_BOUND('',#1789,.T.);
#767=FACE_BOUND('',#1790,.T.);
#768=FACE_BOUND('',#1791,.T.);
#769=FACE_BOUND('',#1792,.T.);
#770=FACE_BOUND('',#1793,.T.);
#771=FACE_BOUND('',#1794,.T.);
#772=FACE_BOUND('',#1795,.T.);
#773=FACE_BOUND('',#1796,.T.);
#774=FACE_BOUND('',#1797,.T.);
#775=FACE_BOUND('',#1798,.T.);
#776=FACE_BOUND('',#1799,.T.);
#777=FACE_BOUND('',#1801,.T.);
#778=FACE_BOUND('',#1802,.T.);
#779=FACE_BOUND('',#1803,.T.);
#780=FACE_BOUND('',#1804,.T.);
#781=FACE_BOUND('',#1805,.T.);
#782=FACE_BOUND('',#1806,.T.);
#783=FACE_BOUND('',#1807,.T.);
#784=FACE_BOUND('',#1808,.T.);
#785=FACE_BOUND('',#1809,.T.);
#786=FACE_BOUND('',#1810,.T.);
#787=FACE_BOUND('',#1811,.T.);
#788=FACE_BOUND('',#1812,.T.);
#789=FACE_BOUND('',#1813,.T.);
#790=FACE_BOUND('',#1814,.T.);
#791=FACE_BOUND('',#1815,.T.);
#792=FACE_BOUND('',#1816,.T.);
#793=FACE_BOUND('',#1817,.T.);
#794=FACE_BOUND('',#1818,.T.);
#795=FACE_BOUND('',#1819,.T.);
#796=FACE_BOUND('',#1820,.T.);
#797=FACE_BOUND('',#1835,.T.);
#798=FACE_BOUND('',#1838,.T.);
#799=FACE_BOUND('',#1841,.T.);
#800=FACE_BOUND('',#1844,.T.);
#801=FACE_BOUND('',#1846,.T.);
#802=FACE_BOUND('',#1847,.T.);
#803=FACE_BOUND('',#1848,.T.);
#804=FACE_BOUND('',#1849,.T.);
#805=FACE_BOUND('',#1850,.T.);
#806=FACE_BOUND('',#1859,.T.);
#807=FACE_BOUND('',#1861,.T.);
#808=FACE_BOUND('',#1862,.T.);
#809=FACE_BOUND('',#1863,.T.);
#810=FACE_BOUND('',#1864,.T.);
#811=FACE_BOUND('',#1865,.T.);
#812=FACE_BOUND('',#1872,.T.);
#813=FACE_BOUND('',#1876,.T.);
#814=FACE_BOUND('',#1877,.T.);
#815=FACE_BOUND('',#1878,.T.);
#816=FACE_BOUND('',#1879,.T.);
#817=FACE_BOUND('',#1880,.T.);
#818=FACE_BOUND('',#1882,.T.);
#819=FACE_BOUND('',#1883,.T.);
#820=FACE_BOUND('',#1884,.T.);
#821=FACE_BOUND('',#1885,.T.);
#822=FACE_BOUND('',#1886,.T.);
#823=FACE_BOUND('',#1901,.T.);
#824=FACE_BOUND('',#1909,.T.);
#825=FACE_BOUND('',#1912,.T.);
#826=FACE_BOUND('',#1917,.T.);
#827=FACE_BOUND('',#1922,.T.);
#828=FACE_BOUND('',#1953,.T.);
#829=FACE_BOUND('',#1956,.T.);
#830=FACE_BOUND('',#1959,.T.);
#831=FACE_BOUND('',#1962,.T.);
#832=FACE_BOUND('',#1965,.T.);
#833=FACE_BOUND('',#1986,.T.);
#834=FACE_BOUND('',#1990,.T.);
#835=FACE_BOUND('',#1991,.T.);
#836=FACE_BOUND('',#1992,.T.);
#837=FACE_BOUND('',#2008,.T.);
#838=FACE_BOUND('',#2009,.T.);
#839=FACE_BOUND('',#2010,.T.);
#840=FACE_BOUND('',#2011,.T.);
#841=FACE_BOUND('',#2012,.T.);
#842=FACE_BOUND('',#2013,.T.);
#843=FACE_BOUND('',#2014,.T.);
#844=FACE_BOUND('',#2015,.T.);
#845=FACE_BOUND('',#2016,.T.);
#846=FACE_BOUND('',#2017,.T.);
#847=FACE_BOUND('',#2018,.T.);
#848=FACE_BOUND('',#2019,.T.);
#849=FACE_BOUND('',#2021,.T.);
#850=FACE_BOUND('',#2022,.T.);
#851=FACE_BOUND('',#2023,.T.);
#852=FACE_BOUND('',#2024,.T.);
#853=FACE_BOUND('',#2025,.T.);
#854=FACE_BOUND('',#2026,.T.);
#855=FACE_BOUND('',#2027,.T.);
#856=FACE_BOUND('',#2028,.T.);
#857=FACE_BOUND('',#2029,.T.);
#858=FACE_BOUND('',#2030,.T.);
#859=FACE_BOUND('',#2031,.T.);
#860=FACE_BOUND('',#2032,.T.);
#861=FACE_BOUND('',#2037,.T.);
#862=FACE_BOUND('',#2039,.T.);
#863=FACE_BOUND('',#2041,.T.);
#864=FACE_BOUND('',#2043,.T.);
#865=FACE_BOUND('',#2049,.T.);
#866=FACE_BOUND('',#2070,.T.);
#867=FACE_BOUND('',#2085,.T.);
#868=FACE_BOUND('',#2087,.T.);
#869=FACE_BOUND('',#2092,.T.);
#870=FACE_BOUND('',#2094,.T.);
#871=FACE_BOUND('',#2100,.T.);
#872=FACE_BOUND('',#2101,.T.);
#873=FACE_BOUND('',#2102,.T.);
#874=FACE_BOUND('',#2103,.T.);
#875=FACE_BOUND('',#2104,.T.);
#876=FACE_BOUND('',#2105,.T.);
#877=FACE_BOUND('',#2107,.T.);
#878=FACE_BOUND('',#2108,.T.);
#879=FACE_BOUND('',#2109,.T.);
#880=FACE_BOUND('',#2110,.T.);
#881=FACE_BOUND('',#2114,.T.);
#882=FACE_BOUND('',#2119,.T.);
#883=FACE_BOUND('',#2123,.T.);
#884=FACE_BOUND('',#2125,.T.);
#885=FACE_BOUND('',#2129,.T.);
#886=FACE_BOUND('',#2131,.T.);
#887=FACE_BOUND('',#2135,.T.);
#888=FACE_BOUND('',#2137,.T.);
#889=FACE_BOUND('',#2148,.T.);
#890=FACE_BOUND('',#2150,.T.);
#891=FACE_BOUND('',#2155,.T.);
#892=FACE_BOUND('',#2157,.T.);
#893=FACE_BOUND('',#2163,.T.);
#894=FACE_BOUND('',#2164,.T.);
#895=FACE_BOUND('',#2165,.T.);
#896=FACE_BOUND('',#2166,.T.);
#897=FACE_BOUND('',#2167,.T.);
#898=FACE_BOUND('',#2168,.T.);
#899=FACE_BOUND('',#2170,.T.);
#900=FACE_BOUND('',#2171,.T.);
#901=FACE_BOUND('',#2172,.T.);
#902=FACE_BOUND('',#2173,.T.);
#903=FACE_BOUND('',#2177,.T.);
#904=FACE_BOUND('',#2182,.T.);
#905=FACE_BOUND('',#2186,.T.);
#906=FACE_BOUND('',#2188,.T.);
#907=FACE_BOUND('',#2192,.T.);
#908=FACE_BOUND('',#2194,.T.);
#909=FACE_BOUND('',#2198,.T.);
#910=FACE_BOUND('',#2200,.T.);
#911=FACE_BOUND('',#2211,.T.);
#912=FACE_BOUND('',#2213,.T.);
#913=FACE_BOUND('',#2218,.T.);
#914=FACE_BOUND('',#2220,.T.);
#915=FACE_BOUND('',#2226,.T.);
#916=FACE_BOUND('',#2227,.T.);
#917=FACE_BOUND('',#2228,.T.);
#918=FACE_BOUND('',#2229,.T.);
#919=FACE_BOUND('',#2230,.T.);
#920=FACE_BOUND('',#2231,.T.);
#921=FACE_BOUND('',#2233,.T.);
#922=FACE_BOUND('',#2234,.T.);
#923=FACE_BOUND('',#2235,.T.);
#924=FACE_BOUND('',#2236,.T.);
#925=FACE_BOUND('',#2240,.T.);
#926=FACE_BOUND('',#2245,.T.);
#927=FACE_BOUND('',#2249,.T.);
#928=FACE_BOUND('',#2251,.T.);
#929=FACE_BOUND('',#2255,.T.);
#930=FACE_BOUND('',#2257,.T.);
#931=FACE_BOUND('',#2261,.T.);
#932=FACE_BOUND('',#2263,.T.);
#933=FACE_BOUND('',#2274,.T.);
#934=FACE_BOUND('',#2276,.T.);
#935=FACE_BOUND('',#2281,.T.);
#936=FACE_BOUND('',#2283,.T.);
#937=FACE_BOUND('',#2289,.T.);
#938=FACE_BOUND('',#2290,.T.);
#939=FACE_BOUND('',#2291,.T.);
#940=FACE_BOUND('',#2292,.T.);
#941=FACE_BOUND('',#2293,.T.);
#942=FACE_BOUND('',#2294,.T.);
#943=FACE_BOUND('',#2296,.T.);
#944=FACE_BOUND('',#2297,.T.);
#945=FACE_BOUND('',#2298,.T.);
#946=FACE_BOUND('',#2299,.T.);
#947=FACE_BOUND('',#2303,.T.);
#948=FACE_BOUND('',#2308,.T.);
#949=FACE_BOUND('',#2312,.T.);
#950=FACE_BOUND('',#2314,.T.);
#951=FACE_BOUND('',#2318,.T.);
#952=FACE_BOUND('',#2320,.T.);
#953=FACE_BOUND('',#2324,.T.);
#954=FACE_BOUND('',#2326,.T.);
#955=FACE_BOUND('',#2341,.T.);
#956=FACE_BOUND('',#2358,.T.);
#957=FACE_BOUND('',#2364,.T.);
#958=FACE_BOUND('',#2366,.T.);
#959=FACE_BOUND('',#2370,.T.);
#960=FACE_BOUND('',#2372,.T.);
#961=FACE_BOUND('',#2376,.T.);
#962=FACE_BOUND('',#2378,.T.);
#963=FACE_BOUND('',#2382,.T.);
#964=FACE_BOUND('',#2384,.T.);
#965=FACE_BOUND('',#2388,.T.);
#966=FACE_BOUND('',#2390,.T.);
#967=FACE_BOUND('',#2394,.T.);
#968=FACE_BOUND('',#2396,.T.);
#969=FACE_BOUND('',#2400,.T.);
#970=FACE_BOUND('',#2402,.T.);
#971=FACE_BOUND('',#2406,.T.);
#972=FACE_BOUND('',#2408,.T.);
#973=FACE_BOUND('',#2412,.T.);
#974=FACE_BOUND('',#2414,.T.);
#975=FACE_BOUND('',#2418,.T.);
#976=FACE_BOUND('',#2420,.T.);
#977=FACE_BOUND('',#2424,.T.);
#978=FACE_BOUND('',#2426,.T.);
#979=FACE_BOUND('',#2430,.T.);
#980=FACE_BOUND('',#2432,.T.);
#981=FACE_BOUND('',#2438,.T.);
#982=FACE_BOUND('',#2441,.T.);
#983=FACE_BOUND('',#2446,.T.);
#984=FACE_BOUND('',#2451,.T.);
#985=FACE_BOUND('',#2479,.T.);
#986=FACE_BOUND('',#2482,.T.);
#987=FACE_BOUND('',#2485,.T.);
#988=FACE_BOUND('',#2488,.T.);
#989=FACE_BOUND('',#2491,.T.);
#990=PLANE('',#9103);
#991=PLANE('',#9104);
#992=PLANE('',#9105);
#993=PLANE('',#9106);
#994=PLANE('',#9107);
#995=PLANE('',#9108);
#996=PLANE('',#9125);
#997=PLANE('',#9129);
#998=PLANE('',#9133);
#999=PLANE('',#9137);
#1000=PLANE('',#9141);
#1001=PLANE('',#9146);
#1002=PLANE('',#9151);
#1003=PLANE('',#9156);
#1004=PLANE('',#9158);
#1005=PLANE('',#9179);
#1006=PLANE('',#9180);
#1007=PLANE('',#9197);
#1008=PLANE('',#9204);
#1009=PLANE('',#9205);
#1010=PLANE('',#9207);
#1011=PLANE('',#9208);
#1012=PLANE('',#9209);
#1013=PLANE('',#9210);
#1014=PLANE('',#9211);
#1015=PLANE('',#9212);
#1016=PLANE('',#9213);
#1017=PLANE('',#9214);
#1018=PLANE('',#9215);
#1019=PLANE('',#9217);
#1020=PLANE('',#9225);
#1021=PLANE('',#9245);
#1022=PLANE('',#9248);
#1023=PLANE('',#9260);
#1024=PLANE('',#9269);
#1025=PLANE('',#9306);
#1026=PLANE('',#9311);
#1027=PLANE('',#9316);
#1028=PLANE('',#9321);
#1029=PLANE('',#9327);
#1030=PLANE('',#9332);
#1031=PLANE('',#9337);
#1032=PLANE('',#9346);
#1033=PLANE('',#9350);
#1034=PLANE('',#9351);
#1035=PLANE('',#9353);
#1036=PLANE('',#9358);
#1037=PLANE('',#9361);
#1038=PLANE('',#9366);
#1039=PLANE('',#9375);
#1040=PLANE('',#9376);
#1041=PLANE('',#9377);
#1042=PLANE('',#9378);
#1043=PLANE('',#9379);
#1044=PLANE('',#9380);
#1045=PLANE('',#9382);
#1046=PLANE('',#9383);
#1047=PLANE('',#9384);
#1048=PLANE('',#9385);
#1049=PLANE('',#9386);
#1050=PLANE('',#9387);
#1051=PLANE('',#9393);
#1052=PLANE('',#9397);
#1053=PLANE('',#9401);
#1054=PLANE('',#9402);
#1055=PLANE('',#9409);
#1056=PLANE('',#9410);
#1057=PLANE('',#9451);
#1058=PLANE('',#9452);
#1059=PLANE('',#9454);
#1060=PLANE('',#9459);
#1061=PLANE('',#9466);
#1062=PLANE('',#9467);
#1063=PLANE('',#9469);
#1064=PLANE('',#9477);
#1065=PLANE('',#9485);
#1066=PLANE('',#9486);
#1067=PLANE('',#9487);
#1068=PLANE('',#9488);
#1069=PLANE('',#9489);
#1070=PLANE('',#9490);
#1071=PLANE('',#9491);
#1072=PLANE('',#9492);
#1073=PLANE('',#9493);
#1074=PLANE('',#9509);
#1075=PLANE('',#9510);
#1076=PLANE('',#9511);
#1077=PLANE('',#9512);
#1078=PLANE('',#9513);
#1079=PLANE('',#9514);
#1080=PLANE('',#9515);
#1081=PLANE('',#9516);
#1082=PLANE('',#9524);
#1083=PLANE('',#9552);
#1084=PLANE('',#9553);
#1085=PLANE('',#9554);
#1086=PLANE('',#9555);
#1087=PLANE('',#9556);
#1088=PLANE('',#9557);
#1089=PLANE('',#9558);
#1090=PLANE('',#9559);
#1091=PLANE('',#9560);
#1092=PLANE('',#9561);
#1093=PLANE('',#9562);
#1094=PLANE('',#9563);
#1095=PLANE('',#9564);
#1096=PLANE('',#9565);
#1097=PLANE('',#9566);
#1098=PLANE('',#9567);
#1099=PLANE('',#9572);
#1100=PLANE('',#9573);
#1101=PLANE('',#9578);
#1102=PLANE('',#9581);
#1103=PLANE('',#9589);
#1104=PLANE('',#9590);
#1105=PLANE('',#9598);
#1106=PLANE('',#9599);
#1107=PLANE('',#9607);
#1108=PLANE('',#9608);
#1109=PLANE('',#9629);
#1110=PLANE('',#9630);
#1111=PLANE('',#9631);
#1112=PLANE('',#9632);
#1113=PLANE('',#9633);
#1114=PLANE('',#9634);
#1115=PLANE('',#9635);
#1116=PLANE('',#9636);
#1117=PLANE('',#9637);
#1118=PLANE('',#9638);
#1119=PLANE('',#9639);
#1120=PLANE('',#9640);
#1121=PLANE('',#9641);
#1122=PLANE('',#9642);
#1123=PLANE('',#9643);
#1124=PLANE('',#9644);
#1125=PLANE('',#9649);
#1126=PLANE('',#9650);
#1127=PLANE('',#9655);
#1128=PLANE('',#9658);
#1129=PLANE('',#9666);
#1130=PLANE('',#9667);
#1131=PLANE('',#9675);
#1132=PLANE('',#9676);
#1133=PLANE('',#9684);
#1134=PLANE('',#9685);
#1135=PLANE('',#9706);
#1136=PLANE('',#9707);
#1137=PLANE('',#9708);
#1138=PLANE('',#9709);
#1139=PLANE('',#9710);
#1140=PLANE('',#9711);
#1141=PLANE('',#9712);
#1142=PLANE('',#9713);
#1143=PLANE('',#9714);
#1144=PLANE('',#9715);
#1145=PLANE('',#9716);
#1146=PLANE('',#9717);
#1147=PLANE('',#9718);
#1148=PLANE('',#9719);
#1149=PLANE('',#9720);
#1150=PLANE('',#9721);
#1151=PLANE('',#9726);
#1152=PLANE('',#9727);
#1153=PLANE('',#9732);
#1154=PLANE('',#9735);
#1155=PLANE('',#9743);
#1156=PLANE('',#9744);
#1157=PLANE('',#9752);
#1158=PLANE('',#9753);
#1159=PLANE('',#9761);
#1160=PLANE('',#9762);
#1161=PLANE('',#9783);
#1162=PLANE('',#9784);
#1163=PLANE('',#9785);
#1164=PLANE('',#9786);
#1165=PLANE('',#9787);
#1166=PLANE('',#9788);
#1167=PLANE('',#9789);
#1168=PLANE('',#9790);
#1169=PLANE('',#9791);
#1170=PLANE('',#9792);
#1171=PLANE('',#9793);
#1172=PLANE('',#9794);
#1173=PLANE('',#9795);
#1174=PLANE('',#9796);
#1175=PLANE('',#9797);
#1176=PLANE('',#9798);
#1177=PLANE('',#9803);
#1178=PLANE('',#9804);
#1179=PLANE('',#9809);
#1180=PLANE('',#9812);
#1181=PLANE('',#9820);
#1182=PLANE('',#9821);
#1183=PLANE('',#9829);
#1184=PLANE('',#9830);
#1185=PLANE('',#9838);
#1186=PLANE('',#9839);
#1187=PLANE('',#9841);
#1188=PLANE('',#9842);
#1189=PLANE('',#9843);
#1190=PLANE('',#9844);
#1191=PLANE('',#9845);
#1192=PLANE('',#9846);
#1193=PLANE('',#9847);
#1194=PLANE('',#9848);
#1195=PLANE('',#9849);
#1196=PLANE('',#9851);
#1197=PLANE('',#9859);
#1198=PLANE('',#9865);
#1199=PLANE('',#9866);
#1200=PLANE('',#9867);
#1201=PLANE('',#9868);
#1202=PLANE('',#9869);
#1203=PLANE('',#9870);
#1204=PLANE('',#9871);
#1205=PLANE('',#9872);
#1206=PLANE('',#9873);
#1207=PLANE('',#9875);
#1208=PLANE('',#9883);
#1209=PLANE('',#9936);
#1210=PLANE('',#9937);
#1211=PLANE('',#9945);
#1212=PLANE('',#9946);
#1213=PLANE('',#9954);
#1214=PLANE('',#9955);
#1215=PLANE('',#9964);
#1216=PLANE('',#9965);
#1217=PLANE('',#9973);
#1218=PLANE('',#9974);
#1219=PLANE('',#9982);
#1220=PLANE('',#9983);
#1221=PLANE('',#9992);
#1222=PLANE('',#9993);
#1223=PLANE('',#10001);
#1224=PLANE('',#10002);
#1225=PLANE('',#10010);
#1226=PLANE('',#10011);
#1227=PLANE('',#10020);
#1228=PLANE('',#10021);
#1229=PLANE('',#10029);
#1230=PLANE('',#10030);
#1231=PLANE('',#10038);
#1232=PLANE('',#10039);
#1233=PLANE('',#10055);
#1234=PLANE('',#10058);
#1235=PLANE('',#10070);
#1236=PLANE('',#10079);
#1237=PLANE('',#10112);
#1238=PLANE('',#10117);
#1239=PLANE('',#10122);
#1240=PLANE('',#10127);
#1241=PLANE('',#10132);
#1242=PLANE('',#10137);
#1243=PLANE('',#10146);
#1244=PLANE('',#10150);
#1245=PLANE('',#10151);
#1246=PLANE('',#10153);
#1247=PLANE('',#10158);
#1248=PLANE('',#10161);
#1249=PLANE('',#10166);
#1250=FACE_OUTER_BOUND('',#1755,.T.);
#1251=FACE_OUTER_BOUND('',#1756,.T.);
#1252=FACE_OUTER_BOUND('',#1757,.T.);
#1253=FACE_OUTER_BOUND('',#1758,.T.);
#1254=FACE_OUTER_BOUND('',#1759,.T.);
#1255=FACE_OUTER_BOUND('',#1760,.T.);
#1256=FACE_OUTER_BOUND('',#1761,.T.);
#1257=FACE_OUTER_BOUND('',#1762,.T.);
#1258=FACE_OUTER_BOUND('',#1763,.T.);
#1259=FACE_OUTER_BOUND('',#1764,.T.);
#1260=FACE_OUTER_BOUND('',#1765,.T.);
#1261=FACE_OUTER_BOUND('',#1766,.T.);
#1262=FACE_OUTER_BOUND('',#1767,.T.);
#1263=FACE_OUTER_BOUND('',#1768,.T.);
#1264=FACE_OUTER_BOUND('',#1769,.T.);
#1265=FACE_OUTER_BOUND('',#1770,.T.);
#1266=FACE_OUTER_BOUND('',#1771,.T.);
#1267=FACE_OUTER_BOUND('',#1772,.T.);
#1268=FACE_OUTER_BOUND('',#1773,.T.);
#1269=FACE_OUTER_BOUND('',#1774,.T.);
#1270=FACE_OUTER_BOUND('',#1775,.T.);
#1271=FACE_OUTER_BOUND('',#1776,.T.);
#1272=FACE_OUTER_BOUND('',#1777,.T.);
#1273=FACE_OUTER_BOUND('',#1778,.T.);
#1274=FACE_OUTER_BOUND('',#1779,.T.);
#1275=FACE_OUTER_BOUND('',#1800,.T.);
#1276=FACE_OUTER_BOUND('',#1821,.T.);
#1277=FACE_OUTER_BOUND('',#1822,.T.);
#1278=FACE_OUTER_BOUND('',#1823,.T.);
#1279=FACE_OUTER_BOUND('',#1824,.T.);
#1280=FACE_OUTER_BOUND('',#1825,.T.);
#1281=FACE_OUTER_BOUND('',#1826,.T.);
#1282=FACE_OUTER_BOUND('',#1827,.T.);
#1283=FACE_OUTER_BOUND('',#1828,.T.);
#1284=FACE_OUTER_BOUND('',#1829,.T.);
#1285=FACE_OUTER_BOUND('',#1830,.T.);
#1286=FACE_OUTER_BOUND('',#1831,.T.);
#1287=FACE_OUTER_BOUND('',#1832,.T.);
#1288=FACE_OUTER_BOUND('',#1833,.T.);
#1289=FACE_OUTER_BOUND('',#1834,.T.);
#1290=FACE_OUTER_BOUND('',#1836,.T.);
#1291=FACE_OUTER_BOUND('',#1837,.T.);
#1292=FACE_OUTER_BOUND('',#1839,.T.);
#1293=FACE_OUTER_BOUND('',#1840,.T.);
#1294=FACE_OUTER_BOUND('',#1842,.T.);
#1295=FACE_OUTER_BOUND('',#1843,.T.);
#1296=FACE_OUTER_BOUND('',#1845,.T.);
#1297=FACE_OUTER_BOUND('',#1851,.T.);
#1298=FACE_OUTER_BOUND('',#1852,.T.);
#1299=FACE_OUTER_BOUND('',#1853,.T.);
#1300=FACE_OUTER_BOUND('',#1854,.T.);
#1301=FACE_OUTER_BOUND('',#1855,.T.);
#1302=FACE_OUTER_BOUND('',#1856,.T.);
#1303=FACE_OUTER_BOUND('',#1857,.T.);
#1304=FACE_OUTER_BOUND('',#1858,.T.);
#1305=FACE_OUTER_BOUND('',#1860,.T.);
#1306=FACE_OUTER_BOUND('',#1866,.T.);
#1307=FACE_OUTER_BOUND('',#1867,.T.);
#1308=FACE_OUTER_BOUND('',#1868,.T.);
#1309=FACE_OUTER_BOUND('',#1869,.T.);
#1310=FACE_OUTER_BOUND('',#1870,.T.);
#1311=FACE_OUTER_BOUND('',#1871,.T.);
#1312=FACE_OUTER_BOUND('',#1873,.T.);
#1313=FACE_OUTER_BOUND('',#1874,.T.);
#1314=FACE_OUTER_BOUND('',#1875,.T.);
#1315=FACE_OUTER_BOUND('',#1881,.T.);
#1316=FACE_OUTER_BOUND('',#1887,.T.);
#1317=FACE_OUTER_BOUND('',#1888,.T.);
#1318=FACE_OUTER_BOUND('',#1889,.T.);
#1319=FACE_OUTER_BOUND('',#1890,.T.);
#1320=FACE_OUTER_BOUND('',#1891,.T.);
#1321=FACE_OUTER_BOUND('',#1892,.T.);
#1322=FACE_OUTER_BOUND('',#1893,.T.);
#1323=FACE_OUTER_BOUND('',#1894,.T.);
#1324=FACE_OUTER_BOUND('',#1895,.T.);
#1325=FACE_OUTER_BOUND('',#1896,.T.);
#1326=FACE_OUTER_BOUND('',#1897,.T.);
#1327=FACE_OUTER_BOUND('',#1898,.T.);
#1328=FACE_OUTER_BOUND('',#1899,.T.);
#1329=FACE_OUTER_BOUND('',#1900,.T.);
#1330=FACE_OUTER_BOUND('',#1902,.T.);
#1331=FACE_OUTER_BOUND('',#1903,.T.);
#1332=FACE_OUTER_BOUND('',#1904,.T.);
#1333=FACE_OUTER_BOUND('',#1905,.T.);
#1334=FACE_OUTER_BOUND('',#1906,.T.);
#1335=FACE_OUTER_BOUND('',#1907,.T.);
#1336=FACE_OUTER_BOUND('',#1908,.T.);
#1337=FACE_OUTER_BOUND('',#1910,.T.);
#1338=FACE_OUTER_BOUND('',#1911,.T.);
#1339=FACE_OUTER_BOUND('',#1913,.T.);
#1340=FACE_OUTER_BOUND('',#1914,.T.);
#1341=FACE_OUTER_BOUND('',#1915,.T.);
#1342=FACE_OUTER_BOUND('',#1916,.T.);
#1343=FACE_OUTER_BOUND('',#1918,.T.);
#1344=FACE_OUTER_BOUND('',#1919,.T.);
#1345=FACE_OUTER_BOUND('',#1920,.T.);
#1346=FACE_OUTER_BOUND('',#1921,.T.);
#1347=FACE_OUTER_BOUND('',#1923,.T.);
#1348=FACE_OUTER_BOUND('',#1924,.T.);
#1349=FACE_OUTER_BOUND('',#1925,.T.);
#1350=FACE_OUTER_BOUND('',#1926,.T.);
#1351=FACE_OUTER_BOUND('',#1927,.T.);
#1352=FACE_OUTER_BOUND('',#1928,.T.);
#1353=FACE_OUTER_BOUND('',#1929,.T.);
#1354=FACE_OUTER_BOUND('',#1930,.T.);
#1355=FACE_OUTER_BOUND('',#1931,.T.);
#1356=FACE_OUTER_BOUND('',#1932,.T.);
#1357=FACE_OUTER_BOUND('',#1933,.T.);
#1358=FACE_OUTER_BOUND('',#1934,.T.);
#1359=FACE_OUTER_BOUND('',#1935,.T.);
#1360=FACE_OUTER_BOUND('',#1936,.T.);
#1361=FACE_OUTER_BOUND('',#1937,.T.);
#1362=FACE_OUTER_BOUND('',#1938,.T.);
#1363=FACE_OUTER_BOUND('',#1939,.T.);
#1364=FACE_OUTER_BOUND('',#1940,.T.);
#1365=FACE_OUTER_BOUND('',#1941,.T.);
#1366=FACE_OUTER_BOUND('',#1942,.T.);
#1367=FACE_OUTER_BOUND('',#1943,.T.);
#1368=FACE_OUTER_BOUND('',#1944,.T.);
#1369=FACE_OUTER_BOUND('',#1945,.T.);
#1370=FACE_OUTER_BOUND('',#1946,.T.);
#1371=FACE_OUTER_BOUND('',#1947,.T.);
#1372=FACE_OUTER_BOUND('',#1948,.T.);
#1373=FACE_OUTER_BOUND('',#1949,.T.);
#1374=FACE_OUTER_BOUND('',#1950,.T.);
#1375=FACE_OUTER_BOUND('',#1951,.T.);
#1376=FACE_OUTER_BOUND('',#1952,.T.);
#1377=FACE_OUTER_BOUND('',#1954,.T.);
#1378=FACE_OUTER_BOUND('',#1955,.T.);
#1379=FACE_OUTER_BOUND('',#1957,.T.);
#1380=FACE_OUTER_BOUND('',#1958,.T.);
#1381=FACE_OUTER_BOUND('',#1960,.T.);
#1382=FACE_OUTER_BOUND('',#1961,.T.);
#1383=FACE_OUTER_BOUND('',#1963,.T.);
#1384=FACE_OUTER_BOUND('',#1964,.T.);
#1385=FACE_OUTER_BOUND('',#1966,.T.);
#1386=FACE_OUTER_BOUND('',#1967,.T.);
#1387=FACE_OUTER_BOUND('',#1968,.T.);
#1388=FACE_OUTER_BOUND('',#1969,.T.);
#1389=FACE_OUTER_BOUND('',#1970,.T.);
#1390=FACE_OUTER_BOUND('',#1971,.T.);
#1391=FACE_OUTER_BOUND('',#1972,.T.);
#1392=FACE_OUTER_BOUND('',#1973,.T.);
#1393=FACE_OUTER_BOUND('',#1974,.T.);
#1394=FACE_OUTER_BOUND('',#1975,.T.);
#1395=FACE_OUTER_BOUND('',#1976,.T.);
#1396=FACE_OUTER_BOUND('',#1977,.T.);
#1397=FACE_OUTER_BOUND('',#1978,.T.);
#1398=FACE_OUTER_BOUND('',#1979,.T.);
#1399=FACE_OUTER_BOUND('',#1980,.T.);
#1400=FACE_OUTER_BOUND('',#1981,.T.);
#1401=FACE_OUTER_BOUND('',#1982,.T.);
#1402=FACE_OUTER_BOUND('',#1983,.T.);
#1403=FACE_OUTER_BOUND('',#1984,.T.);
#1404=FACE_OUTER_BOUND('',#1985,.T.);
#1405=FACE_OUTER_BOUND('',#1987,.T.);
#1406=FACE_OUTER_BOUND('',#1988,.T.);
#1407=FACE_OUTER_BOUND('',#1989,.T.);
#1408=FACE_OUTER_BOUND('',#1993,.T.);
#1409=FACE_OUTER_BOUND('',#1994,.T.);
#1410=FACE_OUTER_BOUND('',#1995,.T.);
#1411=FACE_OUTER_BOUND('',#1996,.T.);
#1412=FACE_OUTER_BOUND('',#1997,.T.);
#1413=FACE_OUTER_BOUND('',#1998,.T.);
#1414=FACE_OUTER_BOUND('',#1999,.T.);
#1415=FACE_OUTER_BOUND('',#2000,.T.);
#1416=FACE_OUTER_BOUND('',#2001,.T.);
#1417=FACE_OUTER_BOUND('',#2002,.T.);
#1418=FACE_OUTER_BOUND('',#2003,.T.);
#1419=FACE_OUTER_BOUND('',#2004,.T.);
#1420=FACE_OUTER_BOUND('',#2005,.T.);
#1421=FACE_OUTER_BOUND('',#2006,.T.);
#1422=FACE_OUTER_BOUND('',#2007,.T.);
#1423=FACE_OUTER_BOUND('',#2020,.T.);
#1424=FACE_OUTER_BOUND('',#2033,.T.);
#1425=FACE_OUTER_BOUND('',#2034,.T.);
#1426=FACE_OUTER_BOUND('',#2035,.T.);
#1427=FACE_OUTER_BOUND('',#2036,.T.);
#1428=FACE_OUTER_BOUND('',#2038,.T.);
#1429=FACE_OUTER_BOUND('',#2040,.T.);
#1430=FACE_OUTER_BOUND('',#2042,.T.);
#1431=FACE_OUTER_BOUND('',#2044,.T.);
#1432=FACE_OUTER_BOUND('',#2045,.T.);
#1433=FACE_OUTER_BOUND('',#2046,.T.);
#1434=FACE_OUTER_BOUND('',#2047,.T.);
#1435=FACE_OUTER_BOUND('',#2048,.T.);
#1436=FACE_OUTER_BOUND('',#2050,.T.);
#1437=FACE_OUTER_BOUND('',#2051,.T.);
#1438=FACE_OUTER_BOUND('',#2052,.T.);
#1439=FACE_OUTER_BOUND('',#2053,.T.);
#1440=FACE_OUTER_BOUND('',#2054,.T.);
#1441=FACE_OUTER_BOUND('',#2055,.T.);
#1442=FACE_OUTER_BOUND('',#2056,.T.);
#1443=FACE_OUTER_BOUND('',#2057,.T.);
#1444=FACE_OUTER_BOUND('',#2058,.T.);
#1445=FACE_OUTER_BOUND('',#2059,.T.);
#1446=FACE_OUTER_BOUND('',#2060,.T.);
#1447=FACE_OUTER_BOUND('',#2061,.T.);
#1448=FACE_OUTER_BOUND('',#2062,.T.);
#1449=FACE_OUTER_BOUND('',#2063,.T.);
#1450=FACE_OUTER_BOUND('',#2064,.T.);
#1451=FACE_OUTER_BOUND('',#2065,.T.);
#1452=FACE_OUTER_BOUND('',#2066,.T.);
#1453=FACE_OUTER_BOUND('',#2067,.T.);
#1454=FACE_OUTER_BOUND('',#2068,.T.);
#1455=FACE_OUTER_BOUND('',#2069,.T.);
#1456=FACE_OUTER_BOUND('',#2071,.T.);
#1457=FACE_OUTER_BOUND('',#2072,.T.);
#1458=FACE_OUTER_BOUND('',#2073,.T.);
#1459=FACE_OUTER_BOUND('',#2074,.T.);
#1460=FACE_OUTER_BOUND('',#2075,.T.);
#1461=FACE_OUTER_BOUND('',#2076,.T.);
#1462=FACE_OUTER_BOUND('',#2077,.T.);
#1463=FACE_OUTER_BOUND('',#2078,.T.);
#1464=FACE_OUTER_BOUND('',#2079,.T.);
#1465=FACE_OUTER_BOUND('',#2080,.T.);
#1466=FACE_OUTER_BOUND('',#2081,.T.);
#1467=FACE_OUTER_BOUND('',#2082,.T.);
#1468=FACE_OUTER_BOUND('',#2083,.T.);
#1469=FACE_OUTER_BOUND('',#2084,.T.);
#1470=FACE_OUTER_BOUND('',#2086,.T.);
#1471=FACE_OUTER_BOUND('',#2088,.T.);
#1472=FACE_OUTER_BOUND('',#2089,.T.);
#1473=FACE_OUTER_BOUND('',#2090,.T.);
#1474=FACE_OUTER_BOUND('',#2091,.T.);
#1475=FACE_OUTER_BOUND('',#2093,.T.);
#1476=FACE_OUTER_BOUND('',#2095,.T.);
#1477=FACE_OUTER_BOUND('',#2096,.T.);
#1478=FACE_OUTER_BOUND('',#2097,.T.);
#1479=FACE_OUTER_BOUND('',#2098,.T.);
#1480=FACE_OUTER_BOUND('',#2099,.T.);
#1481=FACE_OUTER_BOUND('',#2106,.T.);
#1482=FACE_OUTER_BOUND('',#2111,.T.);
#1483=FACE_OUTER_BOUND('',#2112,.T.);
#1484=FACE_OUTER_BOUND('',#2113,.T.);
#1485=FACE_OUTER_BOUND('',#2115,.T.);
#1486=FACE_OUTER_BOUND('',#2116,.T.);
#1487=FACE_OUTER_BOUND('',#2117,.T.);
#1488=FACE_OUTER_BOUND('',#2118,.T.);
#1489=FACE_OUTER_BOUND('',#2120,.T.);
#1490=FACE_OUTER_BOUND('',#2121,.T.);
#1491=FACE_OUTER_BOUND('',#2122,.T.);
#1492=FACE_OUTER_BOUND('',#2124,.T.);
#1493=FACE_OUTER_BOUND('',#2126,.T.);
#1494=FACE_OUTER_BOUND('',#2127,.T.);
#1495=FACE_OUTER_BOUND('',#2128,.T.);
#1496=FACE_OUTER_BOUND('',#2130,.T.);
#1497=FACE_OUTER_BOUND('',#2132,.T.);
#1498=FACE_OUTER_BOUND('',#2133,.T.);
#1499=FACE_OUTER_BOUND('',#2134,.T.);
#1500=FACE_OUTER_BOUND('',#2136,.T.);
#1501=FACE_OUTER_BOUND('',#2138,.T.);
#1502=FACE_OUTER_BOUND('',#2139,.T.);
#1503=FACE_OUTER_BOUND('',#2140,.T.);
#1504=FACE_OUTER_BOUND('',#2141,.T.);
#1505=FACE_OUTER_BOUND('',#2142,.T.);
#1506=FACE_OUTER_BOUND('',#2143,.T.);
#1507=FACE_OUTER_BOUND('',#2144,.T.);
#1508=FACE_OUTER_BOUND('',#2145,.T.);
#1509=FACE_OUTER_BOUND('',#2146,.T.);
#1510=FACE_OUTER_BOUND('',#2147,.T.);
#1511=FACE_OUTER_BOUND('',#2149,.T.);
#1512=FACE_OUTER_BOUND('',#2151,.T.);
#1513=FACE_OUTER_BOUND('',#2152,.T.);
#1514=FACE_OUTER_BOUND('',#2153,.T.);
#1515=FACE_OUTER_BOUND('',#2154,.T.);
#1516=FACE_OUTER_BOUND('',#2156,.T.);
#1517=FACE_OUTER_BOUND('',#2158,.T.);
#1518=FACE_OUTER_BOUND('',#2159,.T.);
#1519=FACE_OUTER_BOUND('',#2160,.T.);
#1520=FACE_OUTER_BOUND('',#2161,.T.);
#1521=FACE_OUTER_BOUND('',#2162,.T.);
#1522=FACE_OUTER_BOUND('',#2169,.T.);
#1523=FACE_OUTER_BOUND('',#2174,.T.);
#1524=FACE_OUTER_BOUND('',#2175,.T.);
#1525=FACE_OUTER_BOUND('',#2176,.T.);
#1526=FACE_OUTER_BOUND('',#2178,.T.);
#1527=FACE_OUTER_BOUND('',#2179,.T.);
#1528=FACE_OUTER_BOUND('',#2180,.T.);
#1529=FACE_OUTER_BOUND('',#2181,.T.);
#1530=FACE_OUTER_BOUND('',#2183,.T.);
#1531=FACE_OUTER_BOUND('',#2184,.T.);
#1532=FACE_OUTER_BOUND('',#2185,.T.);
#1533=FACE_OUTER_BOUND('',#2187,.T.);
#1534=FACE_OUTER_BOUND('',#2189,.T.);
#1535=FACE_OUTER_BOUND('',#2190,.T.);
#1536=FACE_OUTER_BOUND('',#2191,.T.);
#1537=FACE_OUTER_BOUND('',#2193,.T.);
#1538=FACE_OUTER_BOUND('',#2195,.T.);
#1539=FACE_OUTER_BOUND('',#2196,.T.);
#1540=FACE_OUTER_BOUND('',#2197,.T.);
#1541=FACE_OUTER_BOUND('',#2199,.T.);
#1542=FACE_OUTER_BOUND('',#2201,.T.);
#1543=FACE_OUTER_BOUND('',#2202,.T.);
#1544=FACE_OUTER_BOUND('',#2203,.T.);
#1545=FACE_OUTER_BOUND('',#2204,.T.);
#1546=FACE_OUTER_BOUND('',#2205,.T.);
#1547=FACE_OUTER_BOUND('',#2206,.T.);
#1548=FACE_OUTER_BOUND('',#2207,.T.);
#1549=FACE_OUTER_BOUND('',#2208,.T.);
#1550=FACE_OUTER_BOUND('',#2209,.T.);
#1551=FACE_OUTER_BOUND('',#2210,.T.);
#1552=FACE_OUTER_BOUND('',#2212,.T.);
#1553=FACE_OUTER_BOUND('',#2214,.T.);
#1554=FACE_OUTER_BOUND('',#2215,.T.);
#1555=FACE_OUTER_BOUND('',#2216,.T.);
#1556=FACE_OUTER_BOUND('',#2217,.T.);
#1557=FACE_OUTER_BOUND('',#2219,.T.);
#1558=FACE_OUTER_BOUND('',#2221,.T.);
#1559=FACE_OUTER_BOUND('',#2222,.T.);
#1560=FACE_OUTER_BOUND('',#2223,.T.);
#1561=FACE_OUTER_BOUND('',#2224,.T.);
#1562=FACE_OUTER_BOUND('',#2225,.T.);
#1563=FACE_OUTER_BOUND('',#2232,.T.);
#1564=FACE_OUTER_BOUND('',#2237,.T.);
#1565=FACE_OUTER_BOUND('',#2238,.T.);
#1566=FACE_OUTER_BOUND('',#2239,.T.);
#1567=FACE_OUTER_BOUND('',#2241,.T.);
#1568=FACE_OUTER_BOUND('',#2242,.T.);
#1569=FACE_OUTER_BOUND('',#2243,.T.);
#1570=FACE_OUTER_BOUND('',#2244,.T.);
#1571=FACE_OUTER_BOUND('',#2246,.T.);
#1572=FACE_OUTER_BOUND('',#2247,.T.);
#1573=FACE_OUTER_BOUND('',#2248,.T.);
#1574=FACE_OUTER_BOUND('',#2250,.T.);
#1575=FACE_OUTER_BOUND('',#2252,.T.);
#1576=FACE_OUTER_BOUND('',#2253,.T.);
#1577=FACE_OUTER_BOUND('',#2254,.T.);
#1578=FACE_OUTER_BOUND('',#2256,.T.);
#1579=FACE_OUTER_BOUND('',#2258,.T.);
#1580=FACE_OUTER_BOUND('',#2259,.T.);
#1581=FACE_OUTER_BOUND('',#2260,.T.);
#1582=FACE_OUTER_BOUND('',#2262,.T.);
#1583=FACE_OUTER_BOUND('',#2264,.T.);
#1584=FACE_OUTER_BOUND('',#2265,.T.);
#1585=FACE_OUTER_BOUND('',#2266,.T.);
#1586=FACE_OUTER_BOUND('',#2267,.T.);
#1587=FACE_OUTER_BOUND('',#2268,.T.);
#1588=FACE_OUTER_BOUND('',#2269,.T.);
#1589=FACE_OUTER_BOUND('',#2270,.T.);
#1590=FACE_OUTER_BOUND('',#2271,.T.);
#1591=FACE_OUTER_BOUND('',#2272,.T.);
#1592=FACE_OUTER_BOUND('',#2273,.T.);
#1593=FACE_OUTER_BOUND('',#2275,.T.);
#1594=FACE_OUTER_BOUND('',#2277,.T.);
#1595=FACE_OUTER_BOUND('',#2278,.T.);
#1596=FACE_OUTER_BOUND('',#2279,.T.);
#1597=FACE_OUTER_BOUND('',#2280,.T.);
#1598=FACE_OUTER_BOUND('',#2282,.T.);
#1599=FACE_OUTER_BOUND('',#2284,.T.);
#1600=FACE_OUTER_BOUND('',#2285,.T.);
#1601=FACE_OUTER_BOUND('',#2286,.T.);
#1602=FACE_OUTER_BOUND('',#2287,.T.);
#1603=FACE_OUTER_BOUND('',#2288,.T.);
#1604=FACE_OUTER_BOUND('',#2295,.T.);
#1605=FACE_OUTER_BOUND('',#2300,.T.);
#1606=FACE_OUTER_BOUND('',#2301,.T.);
#1607=FACE_OUTER_BOUND('',#2302,.T.);
#1608=FACE_OUTER_BOUND('',#2304,.T.);
#1609=FACE_OUTER_BOUND('',#2305,.T.);
#1610=FACE_OUTER_BOUND('',#2306,.T.);
#1611=FACE_OUTER_BOUND('',#2307,.T.);
#1612=FACE_OUTER_BOUND('',#2309,.T.);
#1613=FACE_OUTER_BOUND('',#2310,.T.);
#1614=FACE_OUTER_BOUND('',#2311,.T.);
#1615=FACE_OUTER_BOUND('',#2313,.T.);
#1616=FACE_OUTER_BOUND('',#2315,.T.);
#1617=FACE_OUTER_BOUND('',#2316,.T.);
#1618=FACE_OUTER_BOUND('',#2317,.T.);
#1619=FACE_OUTER_BOUND('',#2319,.T.);
#1620=FACE_OUTER_BOUND('',#2321,.T.);
#1621=FACE_OUTER_BOUND('',#2322,.T.);
#1622=FACE_OUTER_BOUND('',#2323,.T.);
#1623=FACE_OUTER_BOUND('',#2325,.T.);
#1624=FACE_OUTER_BOUND('',#2327,.T.);
#1625=FACE_OUTER_BOUND('',#2328,.T.);
#1626=FACE_OUTER_BOUND('',#2329,.T.);
#1627=FACE_OUTER_BOUND('',#2330,.T.);
#1628=FACE_OUTER_BOUND('',#2331,.T.);
#1629=FACE_OUTER_BOUND('',#2332,.T.);
#1630=FACE_OUTER_BOUND('',#2333,.T.);
#1631=FACE_OUTER_BOUND('',#2334,.T.);
#1632=FACE_OUTER_BOUND('',#2335,.T.);
#1633=FACE_OUTER_BOUND('',#2336,.T.);
#1634=FACE_OUTER_BOUND('',#2337,.T.);
#1635=FACE_OUTER_BOUND('',#2338,.T.);
#1636=FACE_OUTER_BOUND('',#2339,.T.);
#1637=FACE_OUTER_BOUND('',#2340,.T.);
#1638=FACE_OUTER_BOUND('',#2342,.T.);
#1639=FACE_OUTER_BOUND('',#2343,.T.);
#1640=FACE_OUTER_BOUND('',#2344,.T.);
#1641=FACE_OUTER_BOUND('',#2345,.T.);
#1642=FACE_OUTER_BOUND('',#2346,.T.);
#1643=FACE_OUTER_BOUND('',#2347,.T.);
#1644=FACE_OUTER_BOUND('',#2348,.T.);
#1645=FACE_OUTER_BOUND('',#2349,.T.);
#1646=FACE_OUTER_BOUND('',#2350,.T.);
#1647=FACE_OUTER_BOUND('',#2351,.T.);
#1648=FACE_OUTER_BOUND('',#2352,.T.);
#1649=FACE_OUTER_BOUND('',#2353,.T.);
#1650=FACE_OUTER_BOUND('',#2354,.T.);
#1651=FACE_OUTER_BOUND('',#2355,.T.);
#1652=FACE_OUTER_BOUND('',#2356,.T.);
#1653=FACE_OUTER_BOUND('',#2357,.T.);
#1654=FACE_OUTER_BOUND('',#2359,.T.);
#1655=FACE_OUTER_BOUND('',#2360,.T.);
#1656=FACE_OUTER_BOUND('',#2361,.T.);
#1657=FACE_OUTER_BOUND('',#2362,.T.);
#1658=FACE_OUTER_BOUND('',#2363,.T.);
#1659=FACE_OUTER_BOUND('',#2365,.T.);
#1660=FACE_OUTER_BOUND('',#2367,.T.);
#1661=FACE_OUTER_BOUND('',#2368,.T.);
#1662=FACE_OUTER_BOUND('',#2369,.T.);
#1663=FACE_OUTER_BOUND('',#2371,.T.);
#1664=FACE_OUTER_BOUND('',#2373,.T.);
#1665=FACE_OUTER_BOUND('',#2374,.T.);
#1666=FACE_OUTER_BOUND('',#2375,.T.);
#1667=FACE_OUTER_BOUND('',#2377,.T.);
#1668=FACE_OUTER_BOUND('',#2379,.T.);
#1669=FACE_OUTER_BOUND('',#2380,.T.);
#1670=FACE_OUTER_BOUND('',#2381,.T.);
#1671=FACE_OUTER_BOUND('',#2383,.T.);
#1672=FACE_OUTER_BOUND('',#2385,.T.);
#1673=FACE_OUTER_BOUND('',#2386,.T.);
#1674=FACE_OUTER_BOUND('',#2387,.T.);
#1675=FACE_OUTER_BOUND('',#2389,.T.);
#1676=FACE_OUTER_BOUND('',#2391,.T.);
#1677=FACE_OUTER_BOUND('',#2392,.T.);
#1678=FACE_OUTER_BOUND('',#2393,.T.);
#1679=FACE_OUTER_BOUND('',#2395,.T.);
#1680=FACE_OUTER_BOUND('',#2397,.T.);
#1681=FACE_OUTER_BOUND('',#2398,.T.);
#1682=FACE_OUTER_BOUND('',#2399,.T.);
#1683=FACE_OUTER_BOUND('',#2401,.T.);
#1684=FACE_OUTER_BOUND('',#2403,.T.);
#1685=FACE_OUTER_BOUND('',#2404,.T.);
#1686=FACE_OUTER_BOUND('',#2405,.T.);
#1687=FACE_OUTER_BOUND('',#2407,.T.);
#1688=FACE_OUTER_BOUND('',#2409,.T.);
#1689=FACE_OUTER_BOUND('',#2410,.T.);
#1690=FACE_OUTER_BOUND('',#2411,.T.);
#1691=FACE_OUTER_BOUND('',#2413,.T.);
#1692=FACE_OUTER_BOUND('',#2415,.T.);
#1693=FACE_OUTER_BOUND('',#2416,.T.);
#1694=FACE_OUTER_BOUND('',#2417,.T.);
#1695=FACE_OUTER_BOUND('',#2419,.T.);
#1696=FACE_OUTER_BOUND('',#2421,.T.);
#1697=FACE_OUTER_BOUND('',#2422,.T.);
#1698=FACE_OUTER_BOUND('',#2423,.T.);
#1699=FACE_OUTER_BOUND('',#2425,.T.);
#1700=FACE_OUTER_BOUND('',#2427,.T.);
#1701=FACE_OUTER_BOUND('',#2428,.T.);
#1702=FACE_OUTER_BOUND('',#2429,.T.);
#1703=FACE_OUTER_BOUND('',#2431,.T.);
#1704=FACE_OUTER_BOUND('',#2433,.T.);
#1705=FACE_OUTER_BOUND('',#2434,.T.);
#1706=FACE_OUTER_BOUND('',#2435,.T.);
#1707=FACE_OUTER_BOUND('',#2436,.T.);
#1708=FACE_OUTER_BOUND('',#2437,.T.);
#1709=FACE_OUTER_BOUND('',#2439,.T.);
#1710=FACE_OUTER_BOUND('',#2440,.T.);
#1711=FACE_OUTER_BOUND('',#2442,.T.);
#1712=FACE_OUTER_BOUND('',#2443,.T.);
#1713=FACE_OUTER_BOUND('',#2444,.T.);
#1714=FACE_OUTER_BOUND('',#2445,.T.);
#1715=FACE_OUTER_BOUND('',#2447,.T.);
#1716=FACE_OUTER_BOUND('',#2448,.T.);
#1717=FACE_OUTER_BOUND('',#2449,.T.);
#1718=FACE_OUTER_BOUND('',#2450,.T.);
#1719=FACE_OUTER_BOUND('',#2452,.T.);
#1720=FACE_OUTER_BOUND('',#2453,.T.);
#1721=FACE_OUTER_BOUND('',#2454,.T.);
#1722=FACE_OUTER_BOUND('',#2455,.T.);
#1723=FACE_OUTER_BOUND('',#2456,.T.);
#1724=FACE_OUTER_BOUND('',#2457,.T.);
#1725=FACE_OUTER_BOUND('',#2458,.T.);
#1726=FACE_OUTER_BOUND('',#2459,.T.);
#1727=FACE_OUTER_BOUND('',#2460,.T.);
#1728=FACE_OUTER_BOUND('',#2461,.T.);
#1729=FACE_OUTER_BOUND('',#2462,.T.);
#1730=FACE_OUTER_BOUND('',#2463,.T.);
#1731=FACE_OUTER_BOUND('',#2464,.T.);
#1732=FACE_OUTER_BOUND('',#2465,.T.);
#1733=FACE_OUTER_BOUND('',#2466,.T.);
#1734=FACE_OUTER_BOUND('',#2467,.T.);
#1735=FACE_OUTER_BOUND('',#2468,.T.);
#1736=FACE_OUTER_BOUND('',#2469,.T.);
#1737=FACE_OUTER_BOUND('',#2470,.T.);
#1738=FACE_OUTER_BOUND('',#2471,.T.);
#1739=FACE_OUTER_BOUND('',#2472,.T.);
#1740=FACE_OUTER_BOUND('',#2473,.T.);
#1741=FACE_OUTER_BOUND('',#2474,.T.);
#1742=FACE_OUTER_BOUND('',#2475,.T.);
#1743=FACE_OUTER_BOUND('',#2476,.T.);
#1744=FACE_OUTER_BOUND('',#2477,.T.);
#1745=FACE_OUTER_BOUND('',#2478,.T.);
#1746=FACE_OUTER_BOUND('',#2480,.T.);
#1747=FACE_OUTER_BOUND('',#2481,.T.);
#1748=FACE_OUTER_BOUND('',#2483,.T.);
#1749=FACE_OUTER_BOUND('',#2484,.T.);
#1750=FACE_OUTER_BOUND('',#2486,.T.);
#1751=FACE_OUTER_BOUND('',#2487,.T.);
#1752=FACE_OUTER_BOUND('',#2489,.T.);
#1753=FACE_OUTER_BOUND('',#2490,.T.);
#1754=FACE_OUTER_BOUND('',#2492,.T.);
#1755=EDGE_LOOP('',(#5645,#5646,#5647,#5648));
#1756=EDGE_LOOP('',(#5649,#5650,#5651,#5652));
#1757=EDGE_LOOP('',(#5653,#5654,#5655,#5656));
#1758=EDGE_LOOP('',(#5657,#5658,#5659,#5660));
#1759=EDGE_LOOP('',(#5661,#5662,#5663,#5664));
#1760=EDGE_LOOP('',(#5665,#5666,#5667,#5668));
#1761=EDGE_LOOP('',(#5669,#5670,#5671,#5672));
#1762=EDGE_LOOP('',(#5673,#5674,#5675,#5676));
#1763=EDGE_LOOP('',(#5677,#5678,#5679,#5680));
#1764=EDGE_LOOP('',(#5681,#5682,#5683,#5684));
#1765=EDGE_LOOP('',(#5685,#5686,#5687,#5688));
#1766=EDGE_LOOP('',(#5689,#5690,#5691,#5692));
#1767=EDGE_LOOP('',(#5693,#5694,#5695,#5696));
#1768=EDGE_LOOP('',(#5697,#5698,#5699,#5700));
#1769=EDGE_LOOP('',(#5701,#5702,#5703,#5704));
#1770=EDGE_LOOP('',(#5705,#5706,#5707,#5708));
#1771=EDGE_LOOP('',(#5709,#5710,#5711,#5712));
#1772=EDGE_LOOP('',(#5713,#5714,#5715,#5716));
#1773=EDGE_LOOP('',(#5717,#5718,#5719,#5720));
#1774=EDGE_LOOP('',(#5721,#5722,#5723,#5724));
#1775=EDGE_LOOP('',(#5725,#5726,#5727,#5728));
#1776=EDGE_LOOP('',(#5729,#5730,#5731,#5732));
#1777=EDGE_LOOP('',(#5733,#5734,#5735,#5736));
#1778=EDGE_LOOP('',(#5737,#5738,#5739,#5740));
#1779=EDGE_LOOP('',(#5741,#5742,#5743,#5744));
#1780=EDGE_LOOP('',(#5745));
#1781=EDGE_LOOP('',(#5746));
#1782=EDGE_LOOP('',(#5747));
#1783=EDGE_LOOP('',(#5748));
#1784=EDGE_LOOP('',(#5749));
#1785=EDGE_LOOP('',(#5750));
#1786=EDGE_LOOP('',(#5751));
#1787=EDGE_LOOP('',(#5752));
#1788=EDGE_LOOP('',(#5753));
#1789=EDGE_LOOP('',(#5754));
#1790=EDGE_LOOP('',(#5755));
#1791=EDGE_LOOP('',(#5756));
#1792=EDGE_LOOP('',(#5757));
#1793=EDGE_LOOP('',(#5758));
#1794=EDGE_LOOP('',(#5759));
#1795=EDGE_LOOP('',(#5760));
#1796=EDGE_LOOP('',(#5761));
#1797=EDGE_LOOP('',(#5762));
#1798=EDGE_LOOP('',(#5763));
#1799=EDGE_LOOP('',(#5764));
#1800=EDGE_LOOP('',(#5765,#5766,#5767,#5768));
#1801=EDGE_LOOP('',(#5769));
#1802=EDGE_LOOP('',(#5770));
#1803=EDGE_LOOP('',(#5771));
#1804=EDGE_LOOP('',(#5772));
#1805=EDGE_LOOP('',(#5773));
#1806=EDGE_LOOP('',(#5774));
#1807=EDGE_LOOP('',(#5775));
#1808=EDGE_LOOP('',(#5776));
#1809=EDGE_LOOP('',(#5777));
#1810=EDGE_LOOP('',(#5778));
#1811=EDGE_LOOP('',(#5779));
#1812=EDGE_LOOP('',(#5780));
#1813=EDGE_LOOP('',(#5781));
#1814=EDGE_LOOP('',(#5782));
#1815=EDGE_LOOP('',(#5783));
#1816=EDGE_LOOP('',(#5784));
#1817=EDGE_LOOP('',(#5785));
#1818=EDGE_LOOP('',(#5786));
#1819=EDGE_LOOP('',(#5787));
#1820=EDGE_LOOP('',(#5788));
#1821=EDGE_LOOP('',(#5789,#5790,#5791,#5792));
#1822=EDGE_LOOP('',(#5793,#5794,#5795,#5796));
#1823=EDGE_LOOP('',(#5797,#5798,#5799,#5800));
#1824=EDGE_LOOP('',(#5801,#5802,#5803,#5804));
#1825=EDGE_LOOP('',(#5805,#5806,#5807,#5808));
#1826=EDGE_LOOP('',(#5809));
#1827=EDGE_LOOP('',(#5810,#5811,#5812,#5813));
#1828=EDGE_LOOP('',(#5814));
#1829=EDGE_LOOP('',(#5815,#5816,#5817,#5818));
#1830=EDGE_LOOP('',(#5819));
#1831=EDGE_LOOP('',(#5820,#5821,#5822,#5823));
#1832=EDGE_LOOP('',(#5824));
#1833=EDGE_LOOP('',(#5825,#5826,#5827,#5828));
#1834=EDGE_LOOP('',(#5829,#5830));
#1835=EDGE_LOOP('',(#5831));
#1836=EDGE_LOOP('',(#5832,#5833,#5834,#5835));
#1837=EDGE_LOOP('',(#5836,#5837));
#1838=EDGE_LOOP('',(#5838));
#1839=EDGE_LOOP('',(#5839,#5840,#5841,#5842));
#1840=EDGE_LOOP('',(#5843,#5844));
#1841=EDGE_LOOP('',(#5845));
#1842=EDGE_LOOP('',(#5846,#5847,#5848,#5849));
#1843=EDGE_LOOP('',(#5850,#5851));
#1844=EDGE_LOOP('',(#5852));
#1845=EDGE_LOOP('',(#5853,#5854,#5855,#5856,#5857,#5858,#5859,#5860,#5861,
#5862,#5863,#5864));
#1846=EDGE_LOOP('',(#5865));
#1847=EDGE_LOOP('',(#5866));
#1848=EDGE_LOOP('',(#5867));
#1849=EDGE_LOOP('',(#5868));
#1850=EDGE_LOOP('',(#5869));
#1851=EDGE_LOOP('',(#5870,#5871,#5872,#5873));
#1852=EDGE_LOOP('',(#5874,#5875,#5876,#5877));
#1853=EDGE_LOOP('',(#5878,#5879,#5880,#5881));
#1854=EDGE_LOOP('',(#5882,#5883,#5884,#5885));
#1855=EDGE_LOOP('',(#5886,#5887,#5888,#5889));
#1856=EDGE_LOOP('',(#5890,#5891,#5892,#5893));
#1857=EDGE_LOOP('',(#5894,#5895,#5896,#5897,#5898,#5899,#5900,#5901,#5902,
#5903,#5904,#5905,#5906,#5907,#5908));
#1858=EDGE_LOOP('',(#5909));
#1859=EDGE_LOOP('',(#5910));
#1860=EDGE_LOOP('',(#5911));
#1861=EDGE_LOOP('',(#5912));
#1862=EDGE_LOOP('',(#5913));
#1863=EDGE_LOOP('',(#5914));
#1864=EDGE_LOOP('',(#5915));
#1865=EDGE_LOOP('',(#5916));
#1866=EDGE_LOOP('',(#5917,#5918,#5919,#5920));
#1867=EDGE_LOOP('',(#5921,#5922,#5923,#5924));
#1868=EDGE_LOOP('',(#5925,#5926,#5927,#5928));
#1869=EDGE_LOOP('',(#5929,#5930,#5931,#5932));
#1870=EDGE_LOOP('',(#5933,#5934,#5935,#5936));
#1871=EDGE_LOOP('',(#5937));
#1872=EDGE_LOOP('',(#5938));
#1873=EDGE_LOOP('',(#5939,#5940,#5941,#5942));
#1874=EDGE_LOOP('',(#5943,#5944,#5945,#5946));
#1875=EDGE_LOOP('',(#5947));
#1876=EDGE_LOOP('',(#5948));
#1877=EDGE_LOOP('',(#5949));
#1878=EDGE_LOOP('',(#5950));
#1879=EDGE_LOOP('',(#5951));
#1880=EDGE_LOOP('',(#5952));
#1881=EDGE_LOOP('',(#5953));
#1882=EDGE_LOOP('',(#5954));
#1883=EDGE_LOOP('',(#5955));
#1884=EDGE_LOOP('',(#5956));
#1885=EDGE_LOOP('',(#5957));
#1886=EDGE_LOOP('',(#5958));
#1887=EDGE_LOOP('',(#5959,#5960,#5961,#5962));
#1888=EDGE_LOOP('',(#5963,#5964,#5965,#5966));
#1889=EDGE_LOOP('',(#5967,#5968,#5969,#5970));
#1890=EDGE_LOOP('',(#5971,#5972,#5973,#5974));
#1891=EDGE_LOOP('',(#5975,#5976,#5977,#5978));
#1892=EDGE_LOOP('',(#5979,#5980,#5981,#5982));
#1893=EDGE_LOOP('',(#5983,#5984,#5985,#5986,#5987,#5988));
#1894=EDGE_LOOP('',(#5989,#5990,#5991,#5992,#5993,#5994));
#1895=EDGE_LOOP('',(#5995));
#1896=EDGE_LOOP('',(#5996));
#1897=EDGE_LOOP('',(#5997,#5998,#5999,#6000));
#1898=EDGE_LOOP('',(#6001,#6002,#6003,#6004));
#1899=EDGE_LOOP('',(#6005,#6006,#6007,#6008));
#1900=EDGE_LOOP('',(#6009));
#1901=EDGE_LOOP('',(#6010));
#1902=EDGE_LOOP('',(#6011,#6012,#6013,#6014));
#1903=EDGE_LOOP('',(#6015,#6016,#6017,#6018));
#1904=EDGE_LOOP('',(#6019,#6020,#6021,#6022,#6023,#6024));
#1905=EDGE_LOOP('',(#6025,#6026,#6027,#6028,#6029));
#1906=EDGE_LOOP('',(#6030,#6031,#6032,#6033));
#1907=EDGE_LOOP('',(#6034,#6035,#6036,#6037));
#1908=EDGE_LOOP('',(#6038));
#1909=EDGE_LOOP('',(#6039));
#1910=EDGE_LOOP('',(#6040,#6041,#6042,#6043,#6044));
#1911=EDGE_LOOP('',(#6045));
#1912=EDGE_LOOP('',(#6046));
#1913=EDGE_LOOP('',(#6047,#6048,#6049,#6050));
#1914=EDGE_LOOP('',(#6051,#6052,#6053,#6054,#6055,#6056));
#1915=EDGE_LOOP('',(#6057,#6058,#6059,#6060,#6061));
#1916=EDGE_LOOP('',(#6062));
#1917=EDGE_LOOP('',(#6063));
#1918=EDGE_LOOP('',(#6064,#6065,#6066,#6067));
#1919=EDGE_LOOP('',(#6068,#6069,#6070,#6071));
#1920=EDGE_LOOP('',(#6072,#6073,#6074,#6075));
#1921=EDGE_LOOP('',(#6076));
#1922=EDGE_LOOP('',(#6077));
#1923=EDGE_LOOP('',(#6078,#6079,#6080,#6081,#6082));
#1924=EDGE_LOOP('',(#6083,#6084));
#1925=EDGE_LOOP('',(#6085,#6086));
#1926=EDGE_LOOP('',(#6087,#6088));
#1927=EDGE_LOOP('',(#6089,#6090));
#1928=EDGE_LOOP('',(#6091,#6092));
#1929=EDGE_LOOP('',(#6093,#6094));
#1930=EDGE_LOOP('',(#6095,#6096));
#1931=EDGE_LOOP('',(#6097,#6098));
#1932=EDGE_LOOP('',(#6099,#6100));
#1933=EDGE_LOOP('',(#6101,#6102,#6103,#6104));
#1934=EDGE_LOOP('',(#6105,#6106,#6107,#6108,#6109,#6110,#6111,#6112,#6113,
#6114,#6115,#6116,#6117,#6118,#6119,#6120,#6121,#6122,#6123,#6124,#6125,
#6126));
#1935=EDGE_LOOP('',(#6127,#6128,#6129,#6130));
#1936=EDGE_LOOP('',(#6131,#6132,#6133,#6134));
#1937=EDGE_LOOP('',(#6135,#6136,#6137,#6138));
#1938=EDGE_LOOP('',(#6139,#6140,#6141,#6142));
#1939=EDGE_LOOP('',(#6143,#6144,#6145,#6146));
#1940=EDGE_LOOP('',(#6147,#6148,#6149,#6150));
#1941=EDGE_LOOP('',(#6151,#6152,#6153,#6154,#6155,#6156));
#1942=EDGE_LOOP('',(#6157,#6158,#6159,#6160));
#1943=EDGE_LOOP('',(#6161,#6162,#6163,#6164));
#1944=EDGE_LOOP('',(#6165,#6166,#6167,#6168));
#1945=EDGE_LOOP('',(#6169,#6170,#6171,#6172));
#1946=EDGE_LOOP('',(#6173,#6174,#6175,#6176));
#1947=EDGE_LOOP('',(#6177,#6178,#6179,#6180));
#1948=EDGE_LOOP('',(#6181,#6182,#6183,#6184));
#1949=EDGE_LOOP('',(#6185,#6186,#6187,#6188,#6189,#6190,#6191,#6192,#6193,
#6194,#6195,#6196,#6197,#6198,#6199,#6200,#6201,#6202,#6203,#6204,#6205,
#6206));
#1950=EDGE_LOOP('',(#6207,#6208,#6209,#6210));
#1951=EDGE_LOOP('',(#6211,#6212,#6213,#6214));
#1952=EDGE_LOOP('',(#6215));
#1953=EDGE_LOOP('',(#6216));
#1954=EDGE_LOOP('',(#6217,#6218,#6219,#6220));
#1955=EDGE_LOOP('',(#6221));
#1956=EDGE_LOOP('',(#6222));
#1957=EDGE_LOOP('',(#6223,#6224,#6225,#6226));
#1958=EDGE_LOOP('',(#6227));
#1959=EDGE_LOOP('',(#6228));
#1960=EDGE_LOOP('',(#6229,#6230,#6231,#6232));
#1961=EDGE_LOOP('',(#6233));
#1962=EDGE_LOOP('',(#6234));
#1963=EDGE_LOOP('',(#6235,#6236,#6237,#6238));
#1964=EDGE_LOOP('',(#6239));
#1965=EDGE_LOOP('',(#6240));
#1966=EDGE_LOOP('',(#6241,#6242,#6243,#6244));
#1967=EDGE_LOOP('',(#6245,#6246,#6247,#6248));
#1968=EDGE_LOOP('',(#6249,#6250,#6251,#6252));
#1969=EDGE_LOOP('',(#6253,#6254,#6255,#6256));
#1970=EDGE_LOOP('',(#6257,#6258,#6259,#6260));
#1971=EDGE_LOOP('',(#6261,#6262,#6263,#6264));
#1972=EDGE_LOOP('',(#6265,#6266,#6267,#6268));
#1973=EDGE_LOOP('',(#6269,#6270,#6271,#6272));
#1974=EDGE_LOOP('',(#6273,#6274,#6275,#6276));
#1975=EDGE_LOOP('',(#6277,#6278,#6279,#6280));
#1976=EDGE_LOOP('',(#6281,#6282,#6283,#6284));
#1977=EDGE_LOOP('',(#6285,#6286,#6287,#6288));
#1978=EDGE_LOOP('',(#6289,#6290,#6291,#6292));
#1979=EDGE_LOOP('',(#6293,#6294,#6295,#6296));
#1980=EDGE_LOOP('',(#6297));
#1981=EDGE_LOOP('',(#6298,#6299,#6300,#6301));
#1982=EDGE_LOOP('',(#6302));
#1983=EDGE_LOOP('',(#6303,#6304,#6305,#6306));
#1984=EDGE_LOOP('',(#6307));
#1985=EDGE_LOOP('',(#6308));
#1986=EDGE_LOOP('',(#6309));
#1987=EDGE_LOOP('',(#6310,#6311,#6312,#6313));
#1988=EDGE_LOOP('',(#6314,#6315,#6316,#6317));
#1989=EDGE_LOOP('',(#6318));
#1990=EDGE_LOOP('',(#6319));
#1991=EDGE_LOOP('',(#6320));
#1992=EDGE_LOOP('',(#6321));
#1993=EDGE_LOOP('',(#6322));
#1994=EDGE_LOOP('',(#6323,#6324,#6325,#6326));
#1995=EDGE_LOOP('',(#6327,#6328,#6329,#6330));
#1996=EDGE_LOOP('',(#6331,#6332,#6333,#6334));
#1997=EDGE_LOOP('',(#6335,#6336,#6337,#6338));
#1998=EDGE_LOOP('',(#6339,#6340,#6341,#6342));
#1999=EDGE_LOOP('',(#6343,#6344,#6345,#6346));
#2000=EDGE_LOOP('',(#6347,#6348,#6349,#6350));
#2001=EDGE_LOOP('',(#6351,#6352,#6353,#6354));
#2002=EDGE_LOOP('',(#6355,#6356,#6357,#6358));
#2003=EDGE_LOOP('',(#6359,#6360,#6361,#6362));
#2004=EDGE_LOOP('',(#6363,#6364,#6365,#6366));
#2005=EDGE_LOOP('',(#6367,#6368,#6369,#6370));
#2006=EDGE_LOOP('',(#6371,#6372,#6373,#6374));
#2007=EDGE_LOOP('',(#6375));
#2008=EDGE_LOOP('',(#6376));
#2009=EDGE_LOOP('',(#6377));
#2010=EDGE_LOOP('',(#6378));
#2011=EDGE_LOOP('',(#6379));
#2012=EDGE_LOOP('',(#6380));
#2013=EDGE_LOOP('',(#6381));
#2014=EDGE_LOOP('',(#6382));
#2015=EDGE_LOOP('',(#6383));
#2016=EDGE_LOOP('',(#6384));
#2017=EDGE_LOOP('',(#6385));
#2018=EDGE_LOOP('',(#6386));
#2019=EDGE_LOOP('',(#6387));
#2020=EDGE_LOOP('',(#6388));
#2021=EDGE_LOOP('',(#6389));
#2022=EDGE_LOOP('',(#6390));
#2023=EDGE_LOOP('',(#6391));
#2024=EDGE_LOOP('',(#6392));
#2025=EDGE_LOOP('',(#6393));
#2026=EDGE_LOOP('',(#6394));
#2027=EDGE_LOOP('',(#6395));
#2028=EDGE_LOOP('',(#6396));
#2029=EDGE_LOOP('',(#6397));
#2030=EDGE_LOOP('',(#6398));
#2031=EDGE_LOOP('',(#6399));
#2032=EDGE_LOOP('',(#6400));
#2033=EDGE_LOOP('',(#6401,#6402,#6403));
#2034=EDGE_LOOP('',(#6404,#6405,#6406,#6407,#6408,#6409,#6410,#6411));
#2035=EDGE_LOOP('',(#6412,#6413));
#2036=EDGE_LOOP('',(#6414,#6415,#6416,#6417));
#2037=EDGE_LOOP('',(#6418,#6419,#6420,#6421));
#2038=EDGE_LOOP('',(#6422,#6423,#6424,#6425));
#2039=EDGE_LOOP('',(#6426));
#2040=EDGE_LOOP('',(#6427));
#2041=EDGE_LOOP('',(#6428));
#2042=EDGE_LOOP('',(#6429));
#2043=EDGE_LOOP('',(#6430));
#2044=EDGE_LOOP('',(#6431));
#2045=EDGE_LOOP('',(#6432,#6433,#6434,#6435));
#2046=EDGE_LOOP('',(#6436,#6437,#6438,#6439));
#2047=EDGE_LOOP('',(#6440,#6441,#6442,#6443));
#2048=EDGE_LOOP('',(#6444));
#2049=EDGE_LOOP('',(#6445));
#2050=EDGE_LOOP('',(#6446,#6447,#6448,#6449));
#2051=EDGE_LOOP('',(#6450,#6451,#6452,#6453));
#2052=EDGE_LOOP('',(#6454,#6455,#6456,#6457));
#2053=EDGE_LOOP('',(#6458));
#2054=EDGE_LOOP('',(#6459,#6460,#6461,#6462));
#2055=EDGE_LOOP('',(#6463,#6464,#6465,#6466));
#2056=EDGE_LOOP('',(#6467,#6468,#6469,#6470));
#2057=EDGE_LOOP('',(#6471,#6472,#6473,#6474));
#2058=EDGE_LOOP('',(#6475,#6476,#6477,#6478));
#2059=EDGE_LOOP('',(#6479,#6480,#6481,#6482));
#2060=EDGE_LOOP('',(#6483,#6484,#6485,#6486,#6487,#6488));
#2061=EDGE_LOOP('',(#6489,#6490,#6491,#6492,#6493,#6494));
#2062=EDGE_LOOP('',(#6495,#6496,#6497,#6498));
#2063=EDGE_LOOP('',(#6499,#6500,#6501,#6502));
#2064=EDGE_LOOP('',(#6503,#6504,#6505,#6506));
#2065=EDGE_LOOP('',(#6507,#6508,#6509,#6510));
#2066=EDGE_LOOP('',(#6511,#6512,#6513,#6514));
#2067=EDGE_LOOP('',(#6515,#6516,#6517,#6518));
#2068=EDGE_LOOP('',(#6519,#6520,#6521,#6522,#6523,#6524));
#2069=EDGE_LOOP('',(#6525));
#2070=EDGE_LOOP('',(#6526,#6527,#6528,#6529,#6530,#6531));
#2071=EDGE_LOOP('',(#6532,#6533,#6534,#6535));
#2072=EDGE_LOOP('',(#6536,#6537,#6538,#6539));
#2073=EDGE_LOOP('',(#6540,#6541,#6542,#6543));
#2074=EDGE_LOOP('',(#6544));
#2075=EDGE_LOOP('',(#6545,#6546,#6547,#6548));
#2076=EDGE_LOOP('',(#6549,#6550,#6551,#6552));
#2077=EDGE_LOOP('',(#6553,#6554,#6555,#6556));
#2078=EDGE_LOOP('',(#6557,#6558,#6559,#6560));
#2079=EDGE_LOOP('',(#6561,#6562,#6563,#6564));
#2080=EDGE_LOOP('',(#6565,#6566,#6567,#6568));
#2081=EDGE_LOOP('',(#6569,#6570,#6571,#6572));
#2082=EDGE_LOOP('',(#6573,#6574,#6575,#6576));
#2083=EDGE_LOOP('',(#6577,#6578,#6579,#6580));
#2084=EDGE_LOOP('',(#6581,#6582,#6583,#6584));
#2085=EDGE_LOOP('',(#6585));
#2086=EDGE_LOOP('',(#6586,#6587,#6588,#6589));
#2087=EDGE_LOOP('',(#6590));
#2088=EDGE_LOOP('',(#6591,#6592,#6593,#6594));
#2089=EDGE_LOOP('',(#6595,#6596,#6597,#6598));
#2090=EDGE_LOOP('',(#6599,#6600,#6601,#6602));
#2091=EDGE_LOOP('',(#6603,#6604,#6605,#6606));
#2092=EDGE_LOOP('',(#6607));
#2093=EDGE_LOOP('',(#6608,#6609,#6610,#6611));
#2094=EDGE_LOOP('',(#6612));
#2095=EDGE_LOOP('',(#6613,#6614,#6615,#6616));
#2096=EDGE_LOOP('',(#6617,#6618,#6619,#6620));
#2097=EDGE_LOOP('',(#6621,#6622,#6623,#6624));
#2098=EDGE_LOOP('',(#6625,#6626,#6627,#6628));
#2099=EDGE_LOOP('',(#6629,#6630,#6631,#6632));
#2100=EDGE_LOOP('',(#6633,#6634,#6635,#6636));
#2101=EDGE_LOOP('',(#6637,#6638,#6639,#6640));
#2102=EDGE_LOOP('',(#6641));
#2103=EDGE_LOOP('',(#6642));
#2104=EDGE_LOOP('',(#6643));
#2105=EDGE_LOOP('',(#6644));
#2106=EDGE_LOOP('',(#6645,#6646,#6647,#6648));
#2107=EDGE_LOOP('',(#6649));
#2108=EDGE_LOOP('',(#6650));
#2109=EDGE_LOOP('',(#6651));
#2110=EDGE_LOOP('',(#6652));
#2111=EDGE_LOOP('',(#6653,#6654,#6655,#6656));
#2112=EDGE_LOOP('',(#6657));
#2113=EDGE_LOOP('',(#6658));
#2114=EDGE_LOOP('',(#6659));
#2115=EDGE_LOOP('',(#6660,#6661,#6662,#6663));
#2116=EDGE_LOOP('',(#6664));
#2117=EDGE_LOOP('',(#6665,#6666,#6667,#6668));
#2118=EDGE_LOOP('',(#6669));
#2119=EDGE_LOOP('',(#6670));
#2120=EDGE_LOOP('',(#6671,#6672,#6673,#6674));
#2121=EDGE_LOOP('',(#6675,#6676,#6677,#6678));
#2122=EDGE_LOOP('',(#6679));
#2123=EDGE_LOOP('',(#6680));
#2124=EDGE_LOOP('',(#6681));
#2125=EDGE_LOOP('',(#6682));
#2126=EDGE_LOOP('',(#6683,#6684,#6685,#6686));
#2127=EDGE_LOOP('',(#6687,#6688,#6689,#6690));
#2128=EDGE_LOOP('',(#6691));
#2129=EDGE_LOOP('',(#6692));
#2130=EDGE_LOOP('',(#6693));
#2131=EDGE_LOOP('',(#6694));
#2132=EDGE_LOOP('',(#6695,#6696,#6697,#6698));
#2133=EDGE_LOOP('',(#6699,#6700,#6701,#6702));
#2134=EDGE_LOOP('',(#6703));
#2135=EDGE_LOOP('',(#6704));
#2136=EDGE_LOOP('',(#6705));
#2137=EDGE_LOOP('',(#6706));
#2138=EDGE_LOOP('',(#6707,#6708,#6709,#6710));
#2139=EDGE_LOOP('',(#6711,#6712,#6713,#6714));
#2140=EDGE_LOOP('',(#6715,#6716,#6717,#6718));
#2141=EDGE_LOOP('',(#6719,#6720,#6721,#6722));
#2142=EDGE_LOOP('',(#6723,#6724,#6725,#6726));
#2143=EDGE_LOOP('',(#6727,#6728,#6729,#6730));
#2144=EDGE_LOOP('',(#6731,#6732,#6733,#6734));
#2145=EDGE_LOOP('',(#6735,#6736,#6737,#6738));
#2146=EDGE_LOOP('',(#6739,#6740,#6741,#6742));
#2147=EDGE_LOOP('',(#6743,#6744,#6745,#6746));
#2148=EDGE_LOOP('',(#6747));
#2149=EDGE_LOOP('',(#6748,#6749,#6750,#6751));
#2150=EDGE_LOOP('',(#6752));
#2151=EDGE_LOOP('',(#6753,#6754,#6755,#6756));
#2152=EDGE_LOOP('',(#6757,#6758,#6759,#6760));
#2153=EDGE_LOOP('',(#6761,#6762,#6763,#6764));
#2154=EDGE_LOOP('',(#6765,#6766,#6767,#6768));
#2155=EDGE_LOOP('',(#6769));
#2156=EDGE_LOOP('',(#6770,#6771,#6772,#6773));
#2157=EDGE_LOOP('',(#6774));
#2158=EDGE_LOOP('',(#6775,#6776,#6777,#6778));
#2159=EDGE_LOOP('',(#6779,#6780,#6781,#6782));
#2160=EDGE_LOOP('',(#6783,#6784,#6785,#6786));
#2161=EDGE_LOOP('',(#6787,#6788,#6789,#6790));
#2162=EDGE_LOOP('',(#6791,#6792,#6793,#6794));
#2163=EDGE_LOOP('',(#6795,#6796,#6797,#6798));
#2164=EDGE_LOOP('',(#6799,#6800,#6801,#6802));
#2165=EDGE_LOOP('',(#6803));
#2166=EDGE_LOOP('',(#6804));
#2167=EDGE_LOOP('',(#6805));
#2168=EDGE_LOOP('',(#6806));
#2169=EDGE_LOOP('',(#6807,#6808,#6809,#6810));
#2170=EDGE_LOOP('',(#6811));
#2171=EDGE_LOOP('',(#6812));
#2172=EDGE_LOOP('',(#6813));
#2173=EDGE_LOOP('',(#6814));
#2174=EDGE_LOOP('',(#6815,#6816,#6817,#6818));
#2175=EDGE_LOOP('',(#6819));
#2176=EDGE_LOOP('',(#6820));
#2177=EDGE_LOOP('',(#6821));
#2178=EDGE_LOOP('',(#6822,#6823,#6824,#6825));
#2179=EDGE_LOOP('',(#6826));
#2180=EDGE_LOOP('',(#6827,#6828,#6829,#6830));
#2181=EDGE_LOOP('',(#6831));
#2182=EDGE_LOOP('',(#6832));
#2183=EDGE_LOOP('',(#6833,#6834,#6835,#6836));
#2184=EDGE_LOOP('',(#6837,#6838,#6839,#6840));
#2185=EDGE_LOOP('',(#6841));
#2186=EDGE_LOOP('',(#6842));
#2187=EDGE_LOOP('',(#6843));
#2188=EDGE_LOOP('',(#6844));
#2189=EDGE_LOOP('',(#6845,#6846,#6847,#6848));
#2190=EDGE_LOOP('',(#6849,#6850,#6851,#6852));
#2191=EDGE_LOOP('',(#6853));
#2192=EDGE_LOOP('',(#6854));
#2193=EDGE_LOOP('',(#6855));
#2194=EDGE_LOOP('',(#6856));
#2195=EDGE_LOOP('',(#6857,#6858,#6859,#6860));
#2196=EDGE_LOOP('',(#6861,#6862,#6863,#6864));
#2197=EDGE_LOOP('',(#6865));
#2198=EDGE_LOOP('',(#6866));
#2199=EDGE_LOOP('',(#6867));
#2200=EDGE_LOOP('',(#6868));
#2201=EDGE_LOOP('',(#6869,#6870,#6871,#6872));
#2202=EDGE_LOOP('',(#6873,#6874,#6875,#6876));
#2203=EDGE_LOOP('',(#6877,#6878,#6879,#6880));
#2204=EDGE_LOOP('',(#6881,#6882,#6883,#6884));
#2205=EDGE_LOOP('',(#6885,#6886,#6887,#6888));
#2206=EDGE_LOOP('',(#6889,#6890,#6891,#6892));
#2207=EDGE_LOOP('',(#6893,#6894,#6895,#6896));
#2208=EDGE_LOOP('',(#6897,#6898,#6899,#6900));
#2209=EDGE_LOOP('',(#6901,#6902,#6903,#6904));
#2210=EDGE_LOOP('',(#6905,#6906,#6907,#6908));
#2211=EDGE_LOOP('',(#6909));
#2212=EDGE_LOOP('',(#6910,#6911,#6912,#6913));
#2213=EDGE_LOOP('',(#6914));
#2214=EDGE_LOOP('',(#6915,#6916,#6917,#6918));
#2215=EDGE_LOOP('',(#6919,#6920,#6921,#6922));
#2216=EDGE_LOOP('',(#6923,#6924,#6925,#6926));
#2217=EDGE_LOOP('',(#6927,#6928,#6929,#6930));
#2218=EDGE_LOOP('',(#6931));
#2219=EDGE_LOOP('',(#6932,#6933,#6934,#6935));
#2220=EDGE_LOOP('',(#6936));
#2221=EDGE_LOOP('',(#6937,#6938,#6939,#6940));
#2222=EDGE_LOOP('',(#6941,#6942,#6943,#6944));
#2223=EDGE_LOOP('',(#6945,#6946,#6947,#6948));
#2224=EDGE_LOOP('',(#6949,#6950,#6951,#6952));
#2225=EDGE_LOOP('',(#6953,#6954,#6955,#6956));
#2226=EDGE_LOOP('',(#6957,#6958,#6959,#6960));
#2227=EDGE_LOOP('',(#6961,#6962,#6963,#6964));
#2228=EDGE_LOOP('',(#6965));
#2229=EDGE_LOOP('',(#6966));
#2230=EDGE_LOOP('',(#6967));
#2231=EDGE_LOOP('',(#6968));
#2232=EDGE_LOOP('',(#6969,#6970,#6971,#6972));
#2233=EDGE_LOOP('',(#6973));
#2234=EDGE_LOOP('',(#6974));
#2235=EDGE_LOOP('',(#6975));
#2236=EDGE_LOOP('',(#6976));
#2237=EDGE_LOOP('',(#6977,#6978,#6979,#6980));
#2238=EDGE_LOOP('',(#6981));
#2239=EDGE_LOOP('',(#6982));
#2240=EDGE_LOOP('',(#6983));
#2241=EDGE_LOOP('',(#6984,#6985,#6986,#6987));
#2242=EDGE_LOOP('',(#6988));
#2243=EDGE_LOOP('',(#6989,#6990,#6991,#6992));
#2244=EDGE_LOOP('',(#6993));
#2245=EDGE_LOOP('',(#6994));
#2246=EDGE_LOOP('',(#6995,#6996,#6997,#6998));
#2247=EDGE_LOOP('',(#6999,#7000,#7001,#7002));
#2248=EDGE_LOOP('',(#7003));
#2249=EDGE_LOOP('',(#7004));
#2250=EDGE_LOOP('',(#7005));
#2251=EDGE_LOOP('',(#7006));
#2252=EDGE_LOOP('',(#7007,#7008,#7009,#7010));
#2253=EDGE_LOOP('',(#7011,#7012,#7013,#7014));
#2254=EDGE_LOOP('',(#7015));
#2255=EDGE_LOOP('',(#7016));
#2256=EDGE_LOOP('',(#7017));
#2257=EDGE_LOOP('',(#7018));
#2258=EDGE_LOOP('',(#7019,#7020,#7021,#7022));
#2259=EDGE_LOOP('',(#7023,#7024,#7025,#7026));
#2260=EDGE_LOOP('',(#7027));
#2261=EDGE_LOOP('',(#7028));
#2262=EDGE_LOOP('',(#7029));
#2263=EDGE_LOOP('',(#7030));
#2264=EDGE_LOOP('',(#7031,#7032,#7033,#7034));
#2265=EDGE_LOOP('',(#7035,#7036,#7037,#7038));
#2266=EDGE_LOOP('',(#7039,#7040,#7041,#7042));
#2267=EDGE_LOOP('',(#7043,#7044,#7045,#7046));
#2268=EDGE_LOOP('',(#7047,#7048,#7049,#7050));
#2269=EDGE_LOOP('',(#7051,#7052,#7053,#7054));
#2270=EDGE_LOOP('',(#7055,#7056,#7057,#7058));
#2271=EDGE_LOOP('',(#7059,#7060,#7061,#7062));
#2272=EDGE_LOOP('',(#7063,#7064,#7065,#7066));
#2273=EDGE_LOOP('',(#7067,#7068,#7069,#7070));
#2274=EDGE_LOOP('',(#7071));
#2275=EDGE_LOOP('',(#7072,#7073,#7074,#7075));
#2276=EDGE_LOOP('',(#7076));
#2277=EDGE_LOOP('',(#7077,#7078,#7079,#7080));
#2278=EDGE_LOOP('',(#7081,#7082,#7083,#7084));
#2279=EDGE_LOOP('',(#7085,#7086,#7087,#7088));
#2280=EDGE_LOOP('',(#7089,#7090,#7091,#7092));
#2281=EDGE_LOOP('',(#7093));
#2282=EDGE_LOOP('',(#7094,#7095,#7096,#7097));
#2283=EDGE_LOOP('',(#7098));
#2284=EDGE_LOOP('',(#7099,#7100,#7101,#7102));
#2285=EDGE_LOOP('',(#7103,#7104,#7105,#7106));
#2286=EDGE_LOOP('',(#7107,#7108,#7109,#7110));
#2287=EDGE_LOOP('',(#7111,#7112,#7113,#7114));
#2288=EDGE_LOOP('',(#7115,#7116,#7117,#7118));
#2289=EDGE_LOOP('',(#7119,#7120,#7121,#7122));
#2290=EDGE_LOOP('',(#7123,#7124,#7125,#7126));
#2291=EDGE_LOOP('',(#7127));
#2292=EDGE_LOOP('',(#7128));
#2293=EDGE_LOOP('',(#7129));
#2294=EDGE_LOOP('',(#7130));
#2295=EDGE_LOOP('',(#7131,#7132,#7133,#7134));
#2296=EDGE_LOOP('',(#7135));
#2297=EDGE_LOOP('',(#7136));
#2298=EDGE_LOOP('',(#7137));
#2299=EDGE_LOOP('',(#7138));
#2300=EDGE_LOOP('',(#7139,#7140,#7141,#7142));
#2301=EDGE_LOOP('',(#7143));
#2302=EDGE_LOOP('',(#7144));
#2303=EDGE_LOOP('',(#7145));
#2304=EDGE_LOOP('',(#7146,#7147,#7148,#7149));
#2305=EDGE_LOOP('',(#7150));
#2306=EDGE_LOOP('',(#7151,#7152,#7153,#7154));
#2307=EDGE_LOOP('',(#7155));
#2308=EDGE_LOOP('',(#7156));
#2309=EDGE_LOOP('',(#7157,#7158,#7159,#7160));
#2310=EDGE_LOOP('',(#7161,#7162,#7163,#7164));
#2311=EDGE_LOOP('',(#7165));
#2312=EDGE_LOOP('',(#7166));
#2313=EDGE_LOOP('',(#7167));
#2314=EDGE_LOOP('',(#7168));
#2315=EDGE_LOOP('',(#7169,#7170,#7171,#7172));
#2316=EDGE_LOOP('',(#7173,#7174,#7175,#7176));
#2317=EDGE_LOOP('',(#7177));
#2318=EDGE_LOOP('',(#7178));
#2319=EDGE_LOOP('',(#7179));
#2320=EDGE_LOOP('',(#7180));
#2321=EDGE_LOOP('',(#7181,#7182,#7183,#7184));
#2322=EDGE_LOOP('',(#7185,#7186,#7187,#7188));
#2323=EDGE_LOOP('',(#7189));
#2324=EDGE_LOOP('',(#7190));
#2325=EDGE_LOOP('',(#7191));
#2326=EDGE_LOOP('',(#7192));
#2327=EDGE_LOOP('',(#7193,#7194,#7195,#7196));
#2328=EDGE_LOOP('',(#7197,#7198,#7199,#7200));
#2329=EDGE_LOOP('',(#7201,#7202,#7203,#7204));
#2330=EDGE_LOOP('',(#7205,#7206,#7207,#7208));
#2331=EDGE_LOOP('',(#7209,#7210,#7211,#7212));
#2332=EDGE_LOOP('',(#7213,#7214,#7215,#7216));
#2333=EDGE_LOOP('',(#7217,#7218,#7219,#7220,#7221,#7222));
#2334=EDGE_LOOP('',(#7223,#7224,#7225,#7226,#7227,#7228));
#2335=EDGE_LOOP('',(#7229));
#2336=EDGE_LOOP('',(#7230));
#2337=EDGE_LOOP('',(#7231,#7232,#7233,#7234));
#2338=EDGE_LOOP('',(#7235,#7236,#7237,#7238));
#2339=EDGE_LOOP('',(#7239,#7240,#7241,#7242));
#2340=EDGE_LOOP('',(#7243));
#2341=EDGE_LOOP('',(#7244));
#2342=EDGE_LOOP('',(#7245,#7246,#7247,#7248));
#2343=EDGE_LOOP('',(#7249,#7250,#7251,#7252));
#2344=EDGE_LOOP('',(#7253,#7254,#7255,#7256));
#2345=EDGE_LOOP('',(#7257,#7258,#7259,#7260));
#2346=EDGE_LOOP('',(#7261,#7262,#7263,#7264));
#2347=EDGE_LOOP('',(#7265,#7266,#7267,#7268));
#2348=EDGE_LOOP('',(#7269,#7270,#7271,#7272));
#2349=EDGE_LOOP('',(#7273,#7274,#7275,#7276));
#2350=EDGE_LOOP('',(#7277,#7278,#7279,#7280,#7281,#7282));
#2351=EDGE_LOOP('',(#7283,#7284,#7285,#7286,#7287,#7288));
#2352=EDGE_LOOP('',(#7289));
#2353=EDGE_LOOP('',(#7290));
#2354=EDGE_LOOP('',(#7291,#7292,#7293,#7294));
#2355=EDGE_LOOP('',(#7295,#7296,#7297,#7298));
#2356=EDGE_LOOP('',(#7299,#7300,#7301,#7302));
#2357=EDGE_LOOP('',(#7303));
#2358=EDGE_LOOP('',(#7304));
#2359=EDGE_LOOP('',(#7305,#7306,#7307,#7308));
#2360=EDGE_LOOP('',(#7309,#7310,#7311,#7312));
#2361=EDGE_LOOP('',(#7313,#7314,#7315,#7316));
#2362=EDGE_LOOP('',(#7317,#7318,#7319,#7320));
#2363=EDGE_LOOP('',(#7321));
#2364=EDGE_LOOP('',(#7322));
#2365=EDGE_LOOP('',(#7323));
#2366=EDGE_LOOP('',(#7324));
#2367=EDGE_LOOP('',(#7325,#7326,#7327,#7328));
#2368=EDGE_LOOP('',(#7329,#7330,#7331,#7332));
#2369=EDGE_LOOP('',(#7333));
#2370=EDGE_LOOP('',(#7334));
#2371=EDGE_LOOP('',(#7335));
#2372=EDGE_LOOP('',(#7336));
#2373=EDGE_LOOP('',(#7337,#7338,#7339,#7340));
#2374=EDGE_LOOP('',(#7341,#7342,#7343,#7344));
#2375=EDGE_LOOP('',(#7345));
#2376=EDGE_LOOP('',(#7346));
#2377=EDGE_LOOP('',(#7347));
#2378=EDGE_LOOP('',(#7348));
#2379=EDGE_LOOP('',(#7349,#7350,#7351,#7352));
#2380=EDGE_LOOP('',(#7353,#7354,#7355,#7356));
#2381=EDGE_LOOP('',(#7357));
#2382=EDGE_LOOP('',(#7358));
#2383=EDGE_LOOP('',(#7359));
#2384=EDGE_LOOP('',(#7360));
#2385=EDGE_LOOP('',(#7361,#7362,#7363,#7364));
#2386=EDGE_LOOP('',(#7365,#7366,#7367,#7368));
#2387=EDGE_LOOP('',(#7369));
#2388=EDGE_LOOP('',(#7370));
#2389=EDGE_LOOP('',(#7371));
#2390=EDGE_LOOP('',(#7372));
#2391=EDGE_LOOP('',(#7373,#7374,#7375,#7376));
#2392=EDGE_LOOP('',(#7377,#7378,#7379,#7380));
#2393=EDGE_LOOP('',(#7381));
#2394=EDGE_LOOP('',(#7382));
#2395=EDGE_LOOP('',(#7383));
#2396=EDGE_LOOP('',(#7384));
#2397=EDGE_LOOP('',(#7385,#7386,#7387,#7388));
#2398=EDGE_LOOP('',(#7389,#7390,#7391,#7392));
#2399=EDGE_LOOP('',(#7393));
#2400=EDGE_LOOP('',(#7394));
#2401=EDGE_LOOP('',(#7395));
#2402=EDGE_LOOP('',(#7396));
#2403=EDGE_LOOP('',(#7397,#7398,#7399,#7400));
#2404=EDGE_LOOP('',(#7401,#7402,#7403,#7404));
#2405=EDGE_LOOP('',(#7405));
#2406=EDGE_LOOP('',(#7406));
#2407=EDGE_LOOP('',(#7407));
#2408=EDGE_LOOP('',(#7408));
#2409=EDGE_LOOP('',(#7409,#7410,#7411,#7412));
#2410=EDGE_LOOP('',(#7413,#7414,#7415,#7416));
#2411=EDGE_LOOP('',(#7417));
#2412=EDGE_LOOP('',(#7418));
#2413=EDGE_LOOP('',(#7419));
#2414=EDGE_LOOP('',(#7420));
#2415=EDGE_LOOP('',(#7421,#7422,#7423,#7424));
#2416=EDGE_LOOP('',(#7425,#7426,#7427,#7428));
#2417=EDGE_LOOP('',(#7429));
#2418=EDGE_LOOP('',(#7430));
#2419=EDGE_LOOP('',(#7431));
#2420=EDGE_LOOP('',(#7432));
#2421=EDGE_LOOP('',(#7433,#7434,#7435,#7436));
#2422=EDGE_LOOP('',(#7437,#7438,#7439,#7440));
#2423=EDGE_LOOP('',(#7441));
#2424=EDGE_LOOP('',(#7442));
#2425=EDGE_LOOP('',(#7443));
#2426=EDGE_LOOP('',(#7444));
#2427=EDGE_LOOP('',(#7445,#7446,#7447,#7448));
#2428=EDGE_LOOP('',(#7449,#7450,#7451,#7452));
#2429=EDGE_LOOP('',(#7453));
#2430=EDGE_LOOP('',(#7454));
#2431=EDGE_LOOP('',(#7455));
#2432=EDGE_LOOP('',(#7456));
#2433=EDGE_LOOP('',(#7457,#7458,#7459,#7460,#7461,#7462));
#2434=EDGE_LOOP('',(#7463,#7464,#7465,#7466,#7467));
#2435=EDGE_LOOP('',(#7468,#7469,#7470,#7471));
#2436=EDGE_LOOP('',(#7472,#7473,#7474,#7475));
#2437=EDGE_LOOP('',(#7476));
#2438=EDGE_LOOP('',(#7477));
#2439=EDGE_LOOP('',(#7478,#7479,#7480,#7481,#7482));
#2440=EDGE_LOOP('',(#7483));
#2441=EDGE_LOOP('',(#7484));
#2442=EDGE_LOOP('',(#7485,#7486,#7487,#7488));
#2443=EDGE_LOOP('',(#7489,#7490,#7491,#7492,#7493,#7494));
#2444=EDGE_LOOP('',(#7495,#7496,#7497,#7498,#7499));
#2445=EDGE_LOOP('',(#7500));
#2446=EDGE_LOOP('',(#7501));
#2447=EDGE_LOOP('',(#7502,#7503,#7504,#7505));
#2448=EDGE_LOOP('',(#7506,#7507,#7508,#7509));
#2449=EDGE_LOOP('',(#7510,#7511,#7512,#7513));
#2450=EDGE_LOOP('',(#7514));
#2451=EDGE_LOOP('',(#7515));
#2452=EDGE_LOOP('',(#7516,#7517,#7518,#7519,#7520));
#2453=EDGE_LOOP('',(#7521,#7522));
#2454=EDGE_LOOP('',(#7523,#7524));
#2455=EDGE_LOOP('',(#7525,#7526));
#2456=EDGE_LOOP('',(#7527,#7528));
#2457=EDGE_LOOP('',(#7529,#7530));
#2458=EDGE_LOOP('',(#7531,#7532));
#2459=EDGE_LOOP('',(#7533,#7534));
#2460=EDGE_LOOP('',(#7535,#7536));
#2461=EDGE_LOOP('',(#7537,#7538,#7539,#7540));
#2462=EDGE_LOOP('',(#7541,#7542,#7543,#7544,#7545,#7546,#7547,#7548,#7549,
#7550,#7551,#7552,#7553,#7554,#7555,#7556,#7557,#7558,#7559,#7560));
#2463=EDGE_LOOP('',(#7561,#7562,#7563,#7564));
#2464=EDGE_LOOP('',(#7565,#7566,#7567,#7568));
#2465=EDGE_LOOP('',(#7569,#7570,#7571,#7572));
#2466=EDGE_LOOP('',(#7573,#7574,#7575,#7576));
#2467=EDGE_LOOP('',(#7577,#7578,#7579,#7580));
#2468=EDGE_LOOP('',(#7581,#7582,#7583,#7584,#7585,#7586));
#2469=EDGE_LOOP('',(#7587,#7588,#7589,#7590));
#2470=EDGE_LOOP('',(#7591,#7592,#7593,#7594));
#2471=EDGE_LOOP('',(#7595,#7596,#7597,#7598));
#2472=EDGE_LOOP('',(#7599,#7600,#7601,#7602));
#2473=EDGE_LOOP('',(#7603,#7604,#7605,#7606));
#2474=EDGE_LOOP('',(#7607,#7608,#7609,#7610));
#2475=EDGE_LOOP('',(#7611,#7612,#7613,#7614,#7615,#7616,#7617,#7618,#7619,
#7620,#7621,#7622,#7623,#7624,#7625,#7626,#7627,#7628,#7629,#7630));
#2476=EDGE_LOOP('',(#7631,#7632,#7633,#7634));
#2477=EDGE_LOOP('',(#7635,#7636,#7637,#7638));
#2478=EDGE_LOOP('',(#7639));
#2479=EDGE_LOOP('',(#7640));
#2480=EDGE_LOOP('',(#7641,#7642,#7643,#7644));
#2481=EDGE_LOOP('',(#7645));
#2482=EDGE_LOOP('',(#7646));
#2483=EDGE_LOOP('',(#7647,#7648,#7649,#7650));
#2484=EDGE_LOOP('',(#7651));
#2485=EDGE_LOOP('',(#7652));
#2486=EDGE_LOOP('',(#7653,#7654,#7655,#7656));
#2487=EDGE_LOOP('',(#7657));
#2488=EDGE_LOOP('',(#7658));
#2489=EDGE_LOOP('',(#7659,#7660,#7661,#7662));
#2490=EDGE_LOOP('',(#7663));
#2491=EDGE_LOOP('',(#7664));
#2492=EDGE_LOOP('',(#7665,#7666,#7667,#7668));
#2493=LINE('',#13010,#2976);
#2494=LINE('',#13016,#2977);
#2495=LINE('',#13022,#2978);
#2496=LINE('',#13028,#2979);
#2497=LINE('',#13034,#2980);
#2498=LINE('',#13040,#2981);
#2499=LINE('',#13046,#2982);
#2500=LINE('',#13052,#2983);
#2501=LINE('',#13058,#2984);
#2502=LINE('',#13064,#2985);
#2503=LINE('',#13070,#2986);
#2504=LINE('',#13076,#2987);
#2505=LINE('',#13082,#2988);
#2506=LINE('',#13088,#2989);
#2507=LINE('',#13094,#2990);
#2508=LINE('',#13100,#2991);
#2509=LINE('',#13106,#2992);
#2510=LINE('',#13112,#2993);
#2511=LINE('',#13118,#2994);
#2512=LINE('',#13124,#2995);
#2513=LINE('',#13129,#2996);
#2514=LINE('',#13131,#2997);
#2515=LINE('',#13133,#2998);
#2516=LINE('',#13134,#2999);
#2517=LINE('',#13137,#3000);
#2518=LINE('',#13139,#3001);
#2519=LINE('',#13140,#3002);
#2520=LINE('',#13143,#3003);
#2521=LINE('',#13145,#3004);
#2522=LINE('',#13146,#3005);
#2523=LINE('',#13148,#3006);
#2524=LINE('',#13149,#3007);
#2525=LINE('',#13156,#3008);
#2526=LINE('',#13160,#3009);
#2527=LINE('',#13165,#3010);
#2528=LINE('',#13169,#3011);
#2529=LINE('',#13174,#3012);
#2530=LINE('',#13178,#3013);
#2531=LINE('',#13183,#3014);
#2532=LINE('',#13187,#3015);
#2533=LINE('',#13193,#3016);
#2534=LINE('',#13200,#3017);
#2535=LINE('',#13207,#3018);
#2536=LINE('',#13214,#3019);
#2537=LINE('',#13219,#3020);
#2538=LINE('',#13226,#3021);
#2539=LINE('',#13233,#3022);
#2540=LINE('',#13240,#3023);
#2541=LINE('',#13255,#3024);
#2542=LINE('',#13259,#3025);
#2543=LINE('',#13263,#3026);
#2544=LINE('',#13267,#3027);
#2545=LINE('',#13270,#3028);
#2546=LINE('',#13276,#3029);
#2547=LINE('',#13280,#3030);
#2548=LINE('',#13289,#3031);
#2549=LINE('',#13295,#3032);
#2550=LINE('',#13301,#3033);
#2551=LINE('',#13307,#3034);
#2552=LINE('',#13313,#3035);
#2553=LINE('',#13321,#3036);
#2554=LINE('',#13326,#3037);
#2555=LINE('',#13334,#3038);
#2556=LINE('',#13336,#3039);
#2557=LINE('',#13338,#3040);
#2558=LINE('',#13339,#3041);
#2559=LINE('',#13342,#3042);
#2560=LINE('',#13344,#3043);
#2561=LINE('',#13345,#3044);
#2562=LINE('',#13348,#3045);
#2563=LINE('',#13350,#3046);
#2564=LINE('',#13351,#3047);
#2565=LINE('',#13354,#3048);
#2566=LINE('',#13356,#3049);
#2567=LINE('',#13357,#3050);
#2568=LINE('',#13360,#3051);
#2569=LINE('',#13362,#3052);
#2570=LINE('',#13363,#3053);
#2571=LINE('',#13365,#3054);
#2572=LINE('',#13366,#3055);
#2573=LINE('',#13378,#3056);
#2574=LINE('',#13382,#3057);
#2575=LINE('',#13386,#3058);
#2576=LINE('',#13393,#3059);
#2577=LINE('',#13395,#3060);
#2578=LINE('',#13410,#3061);
#2579=LINE('',#13416,#3062);
#2580=LINE('',#13420,#3063);
#2581=LINE('',#13426,#3064);
#2582=LINE('',#13431,#3065);
#2583=LINE('',#13446,#3066);
#2584=LINE('',#13455,#3067);
#2585=LINE('',#13459,#3068);
#2586=LINE('',#13463,#3069);
#2587=LINE('',#13466,#3070);
#2588=LINE('',#13635,#3071);
#2589=LINE('',#13971,#3072);
#2590=LINE('',#14013,#3073);
#2591=LINE('',#14018,#3074);
#2592=LINE('',#14027,#3075);
#2593=LINE('',#14032,#3076);
#2594=LINE('',#14042,#3077);
#2595=LINE('',#14044,#3078);
#2596=LINE('',#14046,#3079);
#2597=LINE('',#14047,#3080);
#2598=LINE('',#14050,#3081);
#2599=LINE('',#14052,#3082);
#2600=LINE('',#14053,#3083);
#2601=LINE('',#14056,#3084);
#2602=LINE('',#14058,#3085);
#2603=LINE('',#14059,#3086);
#2604=LINE('',#14061,#3087);
#2605=LINE('',#14062,#3088);
#2606=LINE('',#14069,#3089);
#2607=LINE('',#14071,#3090);
#2608=LINE('',#14073,#3091);
#2609=LINE('',#14074,#3092);
#2610=LINE('',#14077,#3093);
#2611=LINE('',#14079,#3094);
#2612=LINE('',#14080,#3095);
#2613=LINE('',#14083,#3096);
#2614=LINE('',#14085,#3097);
#2615=LINE('',#14086,#3098);
#2616=LINE('',#14088,#3099);
#2617=LINE('',#14089,#3100);
#2618=LINE('',#14098,#3101);
#2619=LINE('',#14105,#3102);
#2620=LINE('',#14112,#3103);
#2621=LINE('',#14123,#3104);
#2622=LINE('',#14126,#3105);
#2623=LINE('',#14135,#3106);
#2624=LINE('',#14141,#3107);
#2625=LINE('',#14147,#3108);
#2626=LINE('',#14153,#3109);
#2627=LINE('',#14159,#3110);
#2628=LINE('',#14165,#3111);
#2629=LINE('',#14171,#3112);
#2630=LINE('',#14177,#3113);
#2631=LINE('',#14183,#3114);
#2632=LINE('',#14189,#3115);
#2633=LINE('',#14195,#3116);
#2634=LINE('',#14201,#3117);
#2635=LINE('',#14207,#3118);
#2636=LINE('',#14215,#3119);
#2637=LINE('',#14252,#3120);
#2638=LINE('',#14288,#3121);
#2639=LINE('',#14293,#3122);
#2640=LINE('',#14299,#3123);
#2641=LINE('',#14310,#3124);
#2642=LINE('',#14314,#3125);
#2643=LINE('',#14318,#3126);
#2644=LINE('',#14325,#3127);
#2645=LINE('',#14329,#3128);
#2646=LINE('',#14333,#3129);
#2647=LINE('',#14338,#3130);
#2648=LINE('',#14340,#3131);
#2649=LINE('',#14342,#3132);
#2650=LINE('',#14343,#3133);
#2651=LINE('',#14346,#3134);
#2652=LINE('',#14348,#3135);
#2653=LINE('',#14349,#3136);
#2654=LINE('',#14352,#3137);
#2655=LINE('',#14354,#3138);
#2656=LINE('',#14355,#3139);
#2657=LINE('',#14358,#3140);
#2658=LINE('',#14360,#3141);
#2659=LINE('',#14361,#3142);
#2660=LINE('',#14364,#3143);
#2661=LINE('',#14366,#3144);
#2662=LINE('',#14367,#3145);
#2663=LINE('',#14369,#3146);
#2664=LINE('',#14370,#3147);
#2665=LINE('',#14391,#3148);
#2666=LINE('',#14393,#3149);
#2667=LINE('',#14395,#3150);
#2668=LINE('',#14396,#3151);
#2669=LINE('',#14399,#3152);
#2670=LINE('',#14401,#3153);
#2671=LINE('',#14402,#3154);
#2672=LINE('',#14405,#3155);
#2673=LINE('',#14407,#3156);
#2674=LINE('',#14408,#3157);
#2675=LINE('',#14411,#3158);
#2676=LINE('',#14413,#3159);
#2677=LINE('',#14414,#3160);
#2678=LINE('',#14417,#3161);
#2679=LINE('',#14419,#3162);
#2680=LINE('',#14420,#3163);
#2681=LINE('',#14422,#3164);
#2682=LINE('',#14423,#3165);
#2683=LINE('',#14431,#3166);
#2684=LINE('',#14435,#3167);
#2685=LINE('',#14439,#3168);
#2686=LINE('',#14454,#3169);
#2687=LINE('',#14460,#3170);
#2688=LINE('',#14466,#3171);
#2689=LINE('',#14472,#3172);
#2690=LINE('',#14478,#3173);
#2691=LINE('',#14484,#3174);
#2692=LINE('',#14489,#3175);
#2693=LINE('',#14491,#3176);
#2694=LINE('',#14493,#3177);
#2695=LINE('',#14494,#3178);
#2696=LINE('',#14498,#3179);
#2697=LINE('',#14500,#3180);
#2698=LINE('',#14502,#3181);
#2699=LINE('',#14503,#3182);
#2700=LINE('',#14505,#3183);
#2701=LINE('',#14506,#3184);
#2702=LINE('',#14508,#3185);
#2703=LINE('',#14510,#3186);
#2704=LINE('',#14514,#3187);
#2705=LINE('',#14516,#3188);
#2706=LINE('',#14518,#3189);
#2707=LINE('',#14519,#3190);
#2708=LINE('',#14523,#3191);
#2709=LINE('',#14525,#3192);
#2710=LINE('',#14527,#3193);
#2711=LINE('',#14528,#3194);
#2712=LINE('',#14530,#3195);
#2713=LINE('',#14531,#3196);
#2714=LINE('',#14533,#3197);
#2715=LINE('',#14535,#3198);
#2716=LINE('',#14539,#3199);
#2717=LINE('',#14541,#3200);
#2718=LINE('',#14543,#3201);
#2719=LINE('',#14544,#3202);
#2720=LINE('',#14547,#3203);
#2721=LINE('',#14549,#3204);
#2722=LINE('',#14550,#3205);
#2723=LINE('',#14553,#3206);
#2724=LINE('',#14555,#3207);
#2725=LINE('',#14556,#3208);
#2726=LINE('',#14558,#3209);
#2727=LINE('',#14559,#3210);
#2728=LINE('',#14567,#3211);
#2729=LINE('',#14577,#3212);
#2730=LINE('',#14583,#3213);
#2731=LINE('',#14590,#3214);
#2732=LINE('',#14596,#3215);
#2733=LINE('',#14605,#3216);
#2734=LINE('',#14611,#3217);
#2735=LINE('',#14620,#3218);
#2736=LINE('',#14626,#3219);
#2737=LINE('',#14636,#3220);
#2738=LINE('',#14642,#3221);
#2739=LINE('',#14648,#3222);
#2740=LINE('',#14654,#3223);
#2741=LINE('',#14660,#3224);
#2742=LINE('',#14666,#3225);
#2743=LINE('',#14671,#3226);
#2744=LINE('',#14673,#3227);
#2745=LINE('',#14675,#3228);
#2746=LINE('',#14676,#3229);
#2747=LINE('',#14680,#3230);
#2748=LINE('',#14682,#3231);
#2749=LINE('',#14684,#3232);
#2750=LINE('',#14685,#3233);
#2751=LINE('',#14687,#3234);
#2752=LINE('',#14688,#3235);
#2753=LINE('',#14690,#3236);
#2754=LINE('',#14692,#3237);
#2755=LINE('',#14696,#3238);
#2756=LINE('',#14698,#3239);
#2757=LINE('',#14700,#3240);
#2758=LINE('',#14701,#3241);
#2759=LINE('',#14705,#3242);
#2760=LINE('',#14707,#3243);
#2761=LINE('',#14709,#3244);
#2762=LINE('',#14710,#3245);
#2763=LINE('',#14712,#3246);
#2764=LINE('',#14713,#3247);
#2765=LINE('',#14715,#3248);
#2766=LINE('',#14717,#3249);
#2767=LINE('',#14721,#3250);
#2768=LINE('',#14723,#3251);
#2769=LINE('',#14725,#3252);
#2770=LINE('',#14726,#3253);
#2771=LINE('',#14729,#3254);
#2772=LINE('',#14731,#3255);
#2773=LINE('',#14732,#3256);
#2774=LINE('',#14735,#3257);
#2775=LINE('',#14737,#3258);
#2776=LINE('',#14738,#3259);
#2777=LINE('',#14740,#3260);
#2778=LINE('',#14741,#3261);
#2779=LINE('',#14749,#3262);
#2780=LINE('',#14759,#3263);
#2781=LINE('',#14765,#3264);
#2782=LINE('',#14772,#3265);
#2783=LINE('',#14778,#3266);
#2784=LINE('',#14787,#3267);
#2785=LINE('',#14793,#3268);
#2786=LINE('',#14802,#3269);
#2787=LINE('',#14808,#3270);
#2788=LINE('',#14818,#3271);
#2789=LINE('',#14824,#3272);
#2790=LINE('',#14830,#3273);
#2791=LINE('',#14836,#3274);
#2792=LINE('',#14842,#3275);
#2793=LINE('',#14848,#3276);
#2794=LINE('',#14853,#3277);
#2795=LINE('',#14855,#3278);
#2796=LINE('',#14857,#3279);
#2797=LINE('',#14858,#3280);
#2798=LINE('',#14862,#3281);
#2799=LINE('',#14864,#3282);
#2800=LINE('',#14866,#3283);
#2801=LINE('',#14867,#3284);
#2802=LINE('',#14869,#3285);
#2803=LINE('',#14870,#3286);
#2804=LINE('',#14872,#3287);
#2805=LINE('',#14874,#3288);
#2806=LINE('',#14878,#3289);
#2807=LINE('',#14880,#3290);
#2808=LINE('',#14882,#3291);
#2809=LINE('',#14883,#3292);
#2810=LINE('',#14887,#3293);
#2811=LINE('',#14889,#3294);
#2812=LINE('',#14891,#3295);
#2813=LINE('',#14892,#3296);
#2814=LINE('',#14894,#3297);
#2815=LINE('',#14895,#3298);
#2816=LINE('',#14897,#3299);
#2817=LINE('',#14899,#3300);
#2818=LINE('',#14903,#3301);
#2819=LINE('',#14905,#3302);
#2820=LINE('',#14907,#3303);
#2821=LINE('',#14908,#3304);
#2822=LINE('',#14911,#3305);
#2823=LINE('',#14913,#3306);
#2824=LINE('',#14914,#3307);
#2825=LINE('',#14917,#3308);
#2826=LINE('',#14919,#3309);
#2827=LINE('',#14920,#3310);
#2828=LINE('',#14922,#3311);
#2829=LINE('',#14923,#3312);
#2830=LINE('',#14931,#3313);
#2831=LINE('',#14941,#3314);
#2832=LINE('',#14947,#3315);
#2833=LINE('',#14954,#3316);
#2834=LINE('',#14960,#3317);
#2835=LINE('',#14969,#3318);
#2836=LINE('',#14975,#3319);
#2837=LINE('',#14984,#3320);
#2838=LINE('',#14990,#3321);
#2839=LINE('',#15000,#3322);
#2840=LINE('',#15006,#3323);
#2841=LINE('',#15012,#3324);
#2842=LINE('',#15018,#3325);
#2843=LINE('',#15024,#3326);
#2844=LINE('',#15030,#3327);
#2845=LINE('',#15035,#3328);
#2846=LINE('',#15037,#3329);
#2847=LINE('',#15039,#3330);
#2848=LINE('',#15040,#3331);
#2849=LINE('',#15044,#3332);
#2850=LINE('',#15046,#3333);
#2851=LINE('',#15048,#3334);
#2852=LINE('',#15049,#3335);
#2853=LINE('',#15051,#3336);
#2854=LINE('',#15052,#3337);
#2855=LINE('',#15054,#3338);
#2856=LINE('',#15056,#3339);
#2857=LINE('',#15060,#3340);
#2858=LINE('',#15062,#3341);
#2859=LINE('',#15064,#3342);
#2860=LINE('',#15065,#3343);
#2861=LINE('',#15069,#3344);
#2862=LINE('',#15071,#3345);
#2863=LINE('',#15073,#3346);
#2864=LINE('',#15074,#3347);
#2865=LINE('',#15076,#3348);
#2866=LINE('',#15077,#3349);
#2867=LINE('',#15079,#3350);
#2868=LINE('',#15081,#3351);
#2869=LINE('',#15085,#3352);
#2870=LINE('',#15087,#3353);
#2871=LINE('',#15089,#3354);
#2872=LINE('',#15090,#3355);
#2873=LINE('',#15093,#3356);
#2874=LINE('',#15095,#3357);
#2875=LINE('',#15096,#3358);
#2876=LINE('',#15099,#3359);
#2877=LINE('',#15101,#3360);
#2878=LINE('',#15102,#3361);
#2879=LINE('',#15104,#3362);
#2880=LINE('',#15105,#3363);
#2881=LINE('',#15113,#3364);
#2882=LINE('',#15123,#3365);
#2883=LINE('',#15129,#3366);
#2884=LINE('',#15136,#3367);
#2885=LINE('',#15142,#3368);
#2886=LINE('',#15151,#3369);
#2887=LINE('',#15157,#3370);
#2888=LINE('',#15166,#3371);
#2889=LINE('',#15172,#3372);
#2890=LINE('',#15180,#3373);
#2891=LINE('',#15182,#3374);
#2892=LINE('',#15184,#3375);
#2893=LINE('',#15185,#3376);
#2894=LINE('',#15188,#3377);
#2895=LINE('',#15190,#3378);
#2896=LINE('',#15191,#3379);
#2897=LINE('',#15194,#3380);
#2898=LINE('',#15196,#3381);
#2899=LINE('',#15197,#3382);
#2900=LINE('',#15200,#3383);
#2901=LINE('',#15202,#3384);
#2902=LINE('',#15203,#3385);
#2903=LINE('',#15206,#3386);
#2904=LINE('',#15208,#3387);
#2905=LINE('',#15209,#3388);
#2906=LINE('',#15211,#3389);
#2907=LINE('',#15212,#3390);
#2908=LINE('',#15224,#3391);
#2909=LINE('',#15228,#3392);
#2910=LINE('',#15232,#3393);
#2911=LINE('',#15239,#3394);
#2912=LINE('',#15241,#3395);
#2913=LINE('',#15246,#3396);
#2914=LINE('',#15248,#3397);
#2915=LINE('',#15250,#3398);
#2916=LINE('',#15251,#3399);
#2917=LINE('',#15254,#3400);
#2918=LINE('',#15256,#3401);
#2919=LINE('',#15257,#3402);
#2920=LINE('',#15260,#3403);
#2921=LINE('',#15262,#3404);
#2922=LINE('',#15263,#3405);
#2923=LINE('',#15266,#3406);
#2924=LINE('',#15268,#3407);
#2925=LINE('',#15269,#3408);
#2926=LINE('',#15272,#3409);
#2927=LINE('',#15274,#3410);
#2928=LINE('',#15275,#3411);
#2929=LINE('',#15277,#3412);
#2930=LINE('',#15278,#3413);
#2931=LINE('',#15290,#3414);
#2932=LINE('',#15294,#3415);
#2933=LINE('',#15298,#3416);
#2934=LINE('',#15305,#3417);
#2935=LINE('',#15307,#3418);
#2936=LINE('',#15354,#3419);
#2937=LINE('',#15360,#3420);
#2938=LINE('',#15369,#3421);
#2939=LINE('',#15375,#3422);
#2940=LINE('',#15384,#3423);
#2941=LINE('',#15390,#3424);
#2942=LINE('',#15400,#3425);
#2943=LINE('',#15406,#3426);
#2944=LINE('',#15415,#3427);
#2945=LINE('',#15421,#3428);
#2946=LINE('',#15430,#3429);
#2947=LINE('',#15436,#3430);
#2948=LINE('',#15446,#3431);
#2949=LINE('',#15452,#3432);
#2950=LINE('',#15461,#3433);
#2951=LINE('',#15467,#3434);
#2952=LINE('',#15476,#3435);
#2953=LINE('',#15482,#3436);
#2954=LINE('',#15492,#3437);
#2955=LINE('',#15498,#3438);
#2956=LINE('',#15507,#3439);
#2957=LINE('',#15513,#3440);
#2958=LINE('',#15522,#3441);
#2959=LINE('',#15528,#3442);
#2960=LINE('',#15546,#3443);
#2961=LINE('',#15552,#3444);
#2962=LINE('',#15556,#3445);
#2963=LINE('',#15562,#3446);
#2964=LINE('',#15567,#3447);
#2965=LINE('',#15582,#3448);
#2966=LINE('',#15591,#3449);
#2967=LINE('',#15595,#3450);
#2968=LINE('',#15599,#3451);
#2969=LINE('',#15602,#3452);
#2970=LINE('',#15755,#3453);
#2971=LINE('',#16051,#3454);
#2972=LINE('',#16093,#3455);
#2973=LINE('',#16098,#3456);
#2974=LINE('',#16107,#3457);
#2975=LINE('',#16112,#3458);
#2976=VECTOR('',#10210,0.210000000000001);
#2977=VECTOR('',#10217,0.210000000000001);
#2978=VECTOR('',#10224,0.210000000000001);
#2979=VECTOR('',#10231,0.210000000000001);
#2980=VECTOR('',#10238,0.21);
#2981=VECTOR('',#10245,0.21);
#2982=VECTOR('',#10252,0.21);
#2983=VECTOR('',#10259,0.21);
#2984=VECTOR('',#10266,0.210000000000001);
#2985=VECTOR('',#10273,0.210000000000001);
#2986=VECTOR('',#10280,0.210000000000001);
#2987=VECTOR('',#10287,0.210000000000001);
#2988=VECTOR('',#10294,0.21);
#2989=VECTOR('',#10301,0.21);
#2990=VECTOR('',#10308,0.21);
#2991=VECTOR('',#10315,0.21);
#2992=VECTOR('',#10322,0.25);
#2993=VECTOR('',#10329,0.25);
#2994=VECTOR('',#10336,0.25);
#2995=VECTOR('',#10343,0.25);
#2996=VECTOR('',#10348,1.);
#2997=VECTOR('',#10349,1.);
#2998=VECTOR('',#10350,1.);
#2999=VECTOR('',#10351,1.);
#3000=VECTOR('',#10354,1.);
#3001=VECTOR('',#10355,1.);
#3002=VECTOR('',#10356,1.);
#3003=VECTOR('',#10359,1.);
#3004=VECTOR('',#10360,1.);
#3005=VECTOR('',#10361,1.);
#3006=VECTOR('',#10364,1.);
#3007=VECTOR('',#10365,1.);
#3008=VECTOR('',#10374,0.6);
#3009=VECTOR('',#10377,1.);
#3010=VECTOR('',#10382,0.6);
#3011=VECTOR('',#10385,1.);
#3012=VECTOR('',#10390,0.6);
#3013=VECTOR('',#10393,1.);
#3014=VECTOR('',#10398,0.6);
#3015=VECTOR('',#10401,1.);
#3016=VECTOR('',#10408,0.165);
#3017=VECTOR('',#10417,0.165);
#3018=VECTOR('',#10426,0.165);
#3019=VECTOR('',#10435,0.165);
#3020=VECTOR('',#10444,1.);
#3021=VECTOR('',#10455,1.);
#3022=VECTOR('',#10466,1.);
#3023=VECTOR('',#10477,1.);
#3024=VECTOR('',#10500,0.33);
#3025=VECTOR('',#10505,0.33);
#3026=VECTOR('',#10510,0.33);
#3027=VECTOR('',#10515,0.33);
#3028=VECTOR('',#10518,2.6);
#3029=VECTOR('',#10525,2.2);
#3030=VECTOR('',#10530,4.);
#3031=VECTOR('',#10543,0.225);
#3032=VECTOR('',#10550,0.225);
#3033=VECTOR('',#10557,0.225);
#3034=VECTOR('',#10564,0.225);
#3035=VECTOR('',#10571,2.59);
#3036=VECTOR('',#10582,2.);
#3037=VECTOR('',#10587,4.);
#3038=VECTOR('',#10598,1.);
#3039=VECTOR('',#10599,1.);
#3040=VECTOR('',#10600,1.);
#3041=VECTOR('',#10601,1.);
#3042=VECTOR('',#10604,1.);
#3043=VECTOR('',#10605,1.);
#3044=VECTOR('',#10606,1.);
#3045=VECTOR('',#10609,1.);
#3046=VECTOR('',#10610,1.);
#3047=VECTOR('',#10611,1.);
#3048=VECTOR('',#10614,1.);
#3049=VECTOR('',#10615,1.);
#3050=VECTOR('',#10616,1.);
#3051=VECTOR('',#10619,1.);
#3052=VECTOR('',#10620,1.);
#3053=VECTOR('',#10621,1.);
#3054=VECTOR('',#10624,1.);
#3055=VECTOR('',#10625,1.);
#3056=VECTOR('',#10642,0.475);
#3057=VECTOR('',#10647,0.5);
#3058=VECTOR('',#10652,0.485);
#3059=VECTOR('',#10661,0.31);
#3060=VECTOR('',#10664,0.3);
#3061=VECTOR('',#10683,1.88531);
#3062=VECTOR('',#10690,1.25);
#3063=VECTOR('',#10695,1.3);
#3064=VECTOR('',#10704,1.88531);
#3065=VECTOR('',#10711,1.3);
#3066=VECTOR('',#10730,1.96469);
#3067=VECTOR('',#10741,2.55);
#3068=VECTOR('',#10746,2.6);
#3069=VECTOR('',#10751,2.55);
#3070=VECTOR('',#10756,1.96469);
#3071=VECTOR('',#10813,1.956752);
#3072=VECTOR('',#10904,1.893248);
#3073=VECTOR('',#10933,1.95469);
#3074=VECTOR('',#10940,1.90031);
#3075=VECTOR('',#10951,1.95469);
#3076=VECTOR('',#10958,1.90031);
#3077=VECTOR('',#10973,1.);
#3078=VECTOR('',#10974,1.);
#3079=VECTOR('',#10975,1.);
#3080=VECTOR('',#10976,1.);
#3081=VECTOR('',#10979,1.);
#3082=VECTOR('',#10980,1.);
#3083=VECTOR('',#10981,1.);
#3084=VECTOR('',#10984,1.);
#3085=VECTOR('',#10985,1.);
#3086=VECTOR('',#10986,1.);
#3087=VECTOR('',#10989,1.);
#3088=VECTOR('',#10990,1.);
#3089=VECTOR('',#10999,1.);
#3090=VECTOR('',#11000,1.);
#3091=VECTOR('',#11001,1.);
#3092=VECTOR('',#11002,1.);
#3093=VECTOR('',#11005,1.);
#3094=VECTOR('',#11006,1.);
#3095=VECTOR('',#11007,1.);
#3096=VECTOR('',#11010,1.);
#3097=VECTOR('',#11011,1.);
#3098=VECTOR('',#11012,1.);
#3099=VECTOR('',#11015,1.);
#3100=VECTOR('',#11016,1.);
#3101=VECTOR('',#11029,0.165);
#3102=VECTOR('',#11038,0.165);
#3103=VECTOR('',#11047,0.165);
#3104=VECTOR('',#11062,1.75);
#3105=VECTOR('',#11065,1.25);
#3106=VECTOR('',#11078,0.225);
#3107=VECTOR('',#11085,0.225);
#3108=VECTOR('',#11092,0.225);
#3109=VECTOR('',#11099,0.25);
#3110=VECTOR('',#11106,0.25);
#3111=VECTOR('',#11113,0.25);
#3112=VECTOR('',#11120,0.25);
#3113=VECTOR('',#11127,0.25);
#3114=VECTOR('',#11134,0.25);
#3115=VECTOR('',#11141,0.25);
#3116=VECTOR('',#11148,0.25);
#3117=VECTOR('',#11155,0.25);
#3118=VECTOR('',#11162,20.);
#3119=VECTOR('',#11173,1.);
#3120=VECTOR('',#11182,0.21);
#3121=VECTOR('',#11185,1.);
#3122=VECTOR('',#11190,1.255);
#3123=VECTOR('',#11197,1.8);
#3124=VECTOR('',#11214,0.325);
#3125=VECTOR('',#11219,0.35);
#3126=VECTOR('',#11224,0.335);
#3127=VECTOR('',#11233,0.21);
#3128=VECTOR('',#11238,0.2);
#3129=VECTOR('',#11243,0.18);
#3130=VECTOR('',#11248,1.);
#3131=VECTOR('',#11249,1.);
#3132=VECTOR('',#11250,1.);
#3133=VECTOR('',#11251,1.);
#3134=VECTOR('',#11254,1.);
#3135=VECTOR('',#11255,1.);
#3136=VECTOR('',#11256,1.);
#3137=VECTOR('',#11259,1.);
#3138=VECTOR('',#11260,1.);
#3139=VECTOR('',#11261,1.);
#3140=VECTOR('',#11264,1.);
#3141=VECTOR('',#11265,1.);
#3142=VECTOR('',#11266,1.);
#3143=VECTOR('',#11269,1.);
#3144=VECTOR('',#11270,1.);
#3145=VECTOR('',#11271,1.);
#3146=VECTOR('',#11274,1.);
#3147=VECTOR('',#11275,1.);
#3148=VECTOR('',#11312,1.);
#3149=VECTOR('',#11313,1.);
#3150=VECTOR('',#11314,1.);
#3151=VECTOR('',#11315,1.);
#3152=VECTOR('',#11318,1.);
#3153=VECTOR('',#11319,1.);
#3154=VECTOR('',#11320,1.);
#3155=VECTOR('',#11323,1.);
#3156=VECTOR('',#11324,1.);
#3157=VECTOR('',#11325,1.);
#3158=VECTOR('',#11328,1.);
#3159=VECTOR('',#11329,1.);
#3160=VECTOR('',#11330,1.);
#3161=VECTOR('',#11333,1.);
#3162=VECTOR('',#11334,1.);
#3163=VECTOR('',#11335,1.);
#3164=VECTOR('',#11338,1.);
#3165=VECTOR('',#11339,1.);
#3166=VECTOR('',#11350,0.235);
#3167=VECTOR('',#11355,0.25);
#3168=VECTOR('',#11360,0.2125);
#3169=VECTOR('',#11385,0.275);
#3170=VECTOR('',#11392,0.275);
#3171=VECTOR('',#11399,0.275);
#3172=VECTOR('',#11406,0.275);
#3173=VECTOR('',#11413,0.5);
#3174=VECTOR('',#11420,0.5);
#3175=VECTOR('',#11425,1.);
#3176=VECTOR('',#11426,1.);
#3177=VECTOR('',#11427,1.);
#3178=VECTOR('',#11428,1.);
#3179=VECTOR('',#11431,1.);
#3180=VECTOR('',#11432,1.);
#3181=VECTOR('',#11433,1.);
#3182=VECTOR('',#11434,1.);
#3183=VECTOR('',#11437,1.);
#3184=VECTOR('',#11438,1.);
#3185=VECTOR('',#11441,1.);
#3186=VECTOR('',#11444,1.);
#3187=VECTOR('',#11447,1.);
#3188=VECTOR('',#11448,1.);
#3189=VECTOR('',#11449,1.);
#3190=VECTOR('',#11450,1.);
#3191=VECTOR('',#11453,1.);
#3192=VECTOR('',#11454,1.);
#3193=VECTOR('',#11455,1.);
#3194=VECTOR('',#11456,1.);
#3195=VECTOR('',#11459,1.);
#3196=VECTOR('',#11460,1.);
#3197=VECTOR('',#11463,1.);
#3198=VECTOR('',#11466,1.);
#3199=VECTOR('',#11469,1.);
#3200=VECTOR('',#11470,1.);
#3201=VECTOR('',#11471,1.);
#3202=VECTOR('',#11472,1.);
#3203=VECTOR('',#11475,1.);
#3204=VECTOR('',#11476,1.);
#3205=VECTOR('',#11477,1.);
#3206=VECTOR('',#11480,1.);
#3207=VECTOR('',#11481,1.);
#3208=VECTOR('',#11482,1.);
#3209=VECTOR('',#11485,1.);
#3210=VECTOR('',#11486,1.);
#3211=VECTOR('',#11497,0.165);
#3212=VECTOR('',#11510,0.8);
#3213=VECTOR('',#11519,0.5);
#3214=VECTOR('',#11528,0.505);
#3215=VECTOR('',#11535,0.7);
#3216=VECTOR('',#11548,0.505);
#3217=VECTOR('',#11555,0.7);
#3218=VECTOR('',#11568,0.225);
#3219=VECTOR('',#11575,0.8);
#3220=VECTOR('',#11590,0.275);
#3221=VECTOR('',#11597,0.275);
#3222=VECTOR('',#11604,0.275);
#3223=VECTOR('',#11611,0.275);
#3224=VECTOR('',#11618,0.5);
#3225=VECTOR('',#11625,0.5);
#3226=VECTOR('',#11630,1.);
#3227=VECTOR('',#11631,1.);
#3228=VECTOR('',#11632,1.);
#3229=VECTOR('',#11633,1.);
#3230=VECTOR('',#11636,1.);
#3231=VECTOR('',#11637,1.);
#3232=VECTOR('',#11638,1.);
#3233=VECTOR('',#11639,1.);
#3234=VECTOR('',#11642,1.);
#3235=VECTOR('',#11643,1.);
#3236=VECTOR('',#11646,1.);
#3237=VECTOR('',#11649,1.);
#3238=VECTOR('',#11652,1.);
#3239=VECTOR('',#11653,1.);
#3240=VECTOR('',#11654,1.);
#3241=VECTOR('',#11655,1.);
#3242=VECTOR('',#11658,1.);
#3243=VECTOR('',#11659,1.);
#3244=VECTOR('',#11660,1.);
#3245=VECTOR('',#11661,1.);
#3246=VECTOR('',#11664,1.);
#3247=VECTOR('',#11665,1.);
#3248=VECTOR('',#11668,1.);
#3249=VECTOR('',#11671,1.);
#3250=VECTOR('',#11674,1.);
#3251=VECTOR('',#11675,1.);
#3252=VECTOR('',#11676,1.);
#3253=VECTOR('',#11677,1.);
#3254=VECTOR('',#11680,1.);
#3255=VECTOR('',#11681,1.);
#3256=VECTOR('',#11682,1.);
#3257=VECTOR('',#11685,1.);
#3258=VECTOR('',#11686,1.);
#3259=VECTOR('',#11687,1.);
#3260=VECTOR('',#11690,1.);
#3261=VECTOR('',#11691,1.);
#3262=VECTOR('',#11702,0.165);
#3263=VECTOR('',#11715,0.8);
#3264=VECTOR('',#11724,0.5);
#3265=VECTOR('',#11733,0.505);
#3266=VECTOR('',#11740,0.7);
#3267=VECTOR('',#11753,0.505);
#3268=VECTOR('',#11760,0.7);
#3269=VECTOR('',#11773,0.225);
#3270=VECTOR('',#11780,0.8);
#3271=VECTOR('',#11795,0.275);
#3272=VECTOR('',#11802,0.275);
#3273=VECTOR('',#11809,0.275);
#3274=VECTOR('',#11816,0.275);
#3275=VECTOR('',#11823,0.5);
#3276=VECTOR('',#11830,0.5);
#3277=VECTOR('',#11835,1.);
#3278=VECTOR('',#11836,1.);
#3279=VECTOR('',#11837,1.);
#3280=VECTOR('',#11838,1.);
#3281=VECTOR('',#11841,1.);
#3282=VECTOR('',#11842,1.);
#3283=VECTOR('',#11843,1.);
#3284=VECTOR('',#11844,1.);
#3285=VECTOR('',#11847,1.);
#3286=VECTOR('',#11848,1.);
#3287=VECTOR('',#11851,1.);
#3288=VECTOR('',#11854,1.);
#3289=VECTOR('',#11857,1.);
#3290=VECTOR('',#11858,1.);
#3291=VECTOR('',#11859,1.);
#3292=VECTOR('',#11860,1.);
#3293=VECTOR('',#11863,1.);
#3294=VECTOR('',#11864,1.);
#3295=VECTOR('',#11865,1.);
#3296=VECTOR('',#11866,1.);
#3297=VECTOR('',#11869,1.);
#3298=VECTOR('',#11870,1.);
#3299=VECTOR('',#11873,1.);
#3300=VECTOR('',#11876,1.);
#3301=VECTOR('',#11879,1.);
#3302=VECTOR('',#11880,1.);
#3303=VECTOR('',#11881,1.);
#3304=VECTOR('',#11882,1.);
#3305=VECTOR('',#11885,1.);
#3306=VECTOR('',#11886,1.);
#3307=VECTOR('',#11887,1.);
#3308=VECTOR('',#11890,1.);
#3309=VECTOR('',#11891,1.);
#3310=VECTOR('',#11892,1.);
#3311=VECTOR('',#11895,1.);
#3312=VECTOR('',#11896,1.);
#3313=VECTOR('',#11907,0.165);
#3314=VECTOR('',#11920,0.8);
#3315=VECTOR('',#11929,0.5);
#3316=VECTOR('',#11938,0.505);
#3317=VECTOR('',#11945,0.7);
#3318=VECTOR('',#11958,0.505);
#3319=VECTOR('',#11965,0.7);
#3320=VECTOR('',#11978,0.225);
#3321=VECTOR('',#11985,0.8);
#3322=VECTOR('',#12000,0.275);
#3323=VECTOR('',#12007,0.275);
#3324=VECTOR('',#12014,0.275);
#3325=VECTOR('',#12021,0.275);
#3326=VECTOR('',#12028,0.5);
#3327=VECTOR('',#12035,0.5);
#3328=VECTOR('',#12040,1.);
#3329=VECTOR('',#12041,1.);
#3330=VECTOR('',#12042,1.);
#3331=VECTOR('',#12043,1.);
#3332=VECTOR('',#12046,1.);
#3333=VECTOR('',#12047,1.);
#3334=VECTOR('',#12048,1.);
#3335=VECTOR('',#12049,1.);
#3336=VECTOR('',#12052,1.);
#3337=VECTOR('',#12053,1.);
#3338=VECTOR('',#12056,1.);
#3339=VECTOR('',#12059,1.);
#3340=VECTOR('',#12062,1.);
#3341=VECTOR('',#12063,1.);
#3342=VECTOR('',#12064,1.);
#3343=VECTOR('',#12065,1.);
#3344=VECTOR('',#12068,1.);
#3345=VECTOR('',#12069,1.);
#3346=VECTOR('',#12070,1.);
#3347=VECTOR('',#12071,1.);
#3348=VECTOR('',#12074,1.);
#3349=VECTOR('',#12075,1.);
#3350=VECTOR('',#12078,1.);
#3351=VECTOR('',#12081,1.);
#3352=VECTOR('',#12084,1.);
#3353=VECTOR('',#12085,1.);
#3354=VECTOR('',#12086,1.);
#3355=VECTOR('',#12087,1.);
#3356=VECTOR('',#12090,1.);
#3357=VECTOR('',#12091,1.);
#3358=VECTOR('',#12092,1.);
#3359=VECTOR('',#12095,1.);
#3360=VECTOR('',#12096,1.);
#3361=VECTOR('',#12097,1.);
#3362=VECTOR('',#12100,1.);
#3363=VECTOR('',#12101,1.);
#3364=VECTOR('',#12112,0.165);
#3365=VECTOR('',#12125,0.8);
#3366=VECTOR('',#12134,0.5);
#3367=VECTOR('',#12143,0.505);
#3368=VECTOR('',#12150,0.7);
#3369=VECTOR('',#12163,0.505);
#3370=VECTOR('',#12170,0.7);
#3371=VECTOR('',#12183,0.225);
#3372=VECTOR('',#12190,0.8);
#3373=VECTOR('',#12201,1.);
#3374=VECTOR('',#12202,1.);
#3375=VECTOR('',#12203,1.);
#3376=VECTOR('',#12204,1.);
#3377=VECTOR('',#12207,1.);
#3378=VECTOR('',#12208,1.);
#3379=VECTOR('',#12209,1.);
#3380=VECTOR('',#12212,1.);
#3381=VECTOR('',#12213,1.);
#3382=VECTOR('',#12214,1.);
#3383=VECTOR('',#12217,1.);
#3384=VECTOR('',#12218,1.);
#3385=VECTOR('',#12219,1.);
#3386=VECTOR('',#12222,1.);
#3387=VECTOR('',#12223,1.);
#3388=VECTOR('',#12224,1.);
#3389=VECTOR('',#12227,1.);
#3390=VECTOR('',#12228,1.);
#3391=VECTOR('',#12245,0.4);
#3392=VECTOR('',#12250,0.425);
#3393=VECTOR('',#12255,0.41);
#3394=VECTOR('',#12264,0.26);
#3395=VECTOR('',#12267,0.25);
#3396=VECTOR('',#12272,1.);
#3397=VECTOR('',#12273,1.);
#3398=VECTOR('',#12274,1.);
#3399=VECTOR('',#12275,1.);
#3400=VECTOR('',#12278,1.);
#3401=VECTOR('',#12279,1.);
#3402=VECTOR('',#12280,1.);
#3403=VECTOR('',#12283,1.);
#3404=VECTOR('',#12284,1.);
#3405=VECTOR('',#12285,1.);
#3406=VECTOR('',#12288,1.);
#3407=VECTOR('',#12289,1.);
#3408=VECTOR('',#12290,1.);
#3409=VECTOR('',#12293,1.);
#3410=VECTOR('',#12294,1.);
#3411=VECTOR('',#12295,1.);
#3412=VECTOR('',#12298,1.);
#3413=VECTOR('',#12299,1.);
#3414=VECTOR('',#12316,0.325);
#3415=VECTOR('',#12321,0.35);
#3416=VECTOR('',#12326,0.335);
#3417=VECTOR('',#12335,0.21);
#3418=VECTOR('',#12338,0.2);
#3419=VECTOR('',#12427,1.5);
#3420=VECTOR('',#12434,2.);
#3421=VECTOR('',#12447,1.1);
#3422=VECTOR('',#12454,1.5);
#3423=VECTOR('',#12467,1.1);
#3424=VECTOR('',#12474,1.5);
#3425=VECTOR('',#12489,1.5);
#3426=VECTOR('',#12496,2.);
#3427=VECTOR('',#12509,1.1);
#3428=VECTOR('',#12516,1.5);
#3429=VECTOR('',#12529,1.1);
#3430=VECTOR('',#12536,1.5);
#3431=VECTOR('',#12551,1.5);
#3432=VECTOR('',#12558,2.);
#3433=VECTOR('',#12571,1.1);
#3434=VECTOR('',#12578,1.5);
#3435=VECTOR('',#12591,1.1);
#3436=VECTOR('',#12598,1.5);
#3437=VECTOR('',#12613,1.5);
#3438=VECTOR('',#12620,2.);
#3439=VECTOR('',#12633,1.1);
#3440=VECTOR('',#12640,1.5);
#3441=VECTOR('',#12653,1.1);
#3442=VECTOR('',#12660,1.5);
#3443=VECTOR('',#12685,0.976185);
#3444=VECTOR('',#12692,0.5);
#3445=VECTOR('',#12697,0.53);
#3446=VECTOR('',#12706,0.976185);
#3447=VECTOR('',#12713,0.53);
#3448=VECTOR('',#12732,1.023815);
#3449=VECTOR('',#12743,1.47);
#3450=VECTOR('',#12748,1.5);
#3451=VECTOR('',#12753,1.47);
#3452=VECTOR('',#12758,1.023815);
#3453=VECTOR('',#12809,1.019052);
#3454=VECTOR('',#12886,0.980948);
#3455=VECTOR('',#12915,1.013815);
#3456=VECTOR('',#12922,0.991185);
#3457=VECTOR('',#12933,1.013815);
#3458=VECTOR('',#12940,0.991185);
#3459=CIRCLE('',#9044,0.210000000000001);
#3460=CIRCLE('',#9045,0.210000000000001);
#3461=CIRCLE('',#9047,0.210000000000001);
#3462=CIRCLE('',#9048,0.210000000000001);
#3463=CIRCLE('',#9050,0.210000000000001);
#3464=CIRCLE('',#9051,0.210000000000001);
#3465=CIRCLE('',#9053,0.210000000000001);
#3466=CIRCLE('',#9054,0.210000000000001);
#3467=CIRCLE('',#9056,0.21);
#3468=CIRCLE('',#9057,0.21);
#3469=CIRCLE('',#9059,0.21);
#3470=CIRCLE('',#9060,0.21);
#3471=CIRCLE('',#9062,0.21);
#3472=CIRCLE('',#9063,0.21);
#3473=CIRCLE('',#9065,0.21);
#3474=CIRCLE('',#9066,0.21);
#3475=CIRCLE('',#9068,0.210000000000001);
#3476=CIRCLE('',#9069,0.210000000000001);
#3477=CIRCLE('',#9071,0.210000000000001);
#3478=CIRCLE('',#9072,0.210000000000001);
#3479=CIRCLE('',#9074,0.210000000000001);
#3480=CIRCLE('',#9075,0.210000000000001);
#3481=CIRCLE('',#9077,0.210000000000001);
#3482=CIRCLE('',#9078,0.210000000000001);
#3483=CIRCLE('',#9080,0.21);
#3484=CIRCLE('',#9081,0.21);
#3485=CIRCLE('',#9083,0.21);
#3486=CIRCLE('',#9084,0.21);
#3487=CIRCLE('',#9086,0.21);
#3488=CIRCLE('',#9087,0.21);
#3489=CIRCLE('',#9089,0.21);
#3490=CIRCLE('',#9090,0.21);
#3491=CIRCLE('',#9092,0.25);
#3492=CIRCLE('',#9093,0.25);
#3493=CIRCLE('',#9095,0.25);
#3494=CIRCLE('',#9096,0.25);
#3495=CIRCLE('',#9098,0.25);
#3496=CIRCLE('',#9099,0.25);
#3497=CIRCLE('',#9101,0.25);
#3498=CIRCLE('',#9102,0.25);
#3499=CIRCLE('',#9111,0.6);
#3500=CIRCLE('',#9112,0.6);
#3501=CIRCLE('',#9114,0.6);
#3502=CIRCLE('',#9115,0.6);
#3503=CIRCLE('',#9117,0.6);
#3504=CIRCLE('',#9118,0.6);
#3505=CIRCLE('',#9120,0.6);
#3506=CIRCLE('',#9121,0.6);
#3507=CIRCLE('',#9123,0.165);
#3508=CIRCLE('',#9124,0.165);
#3509=CIRCLE('',#9127,0.165);
#3510=CIRCLE('',#9128,0.165);
#3511=CIRCLE('',#9131,0.165);
#3512=CIRCLE('',#9132,0.165);
#3513=CIRCLE('',#9135,0.165);
#3514=CIRCLE('',#9136,0.165);
#3515=CIRCLE('',#9139,0.6);
#3516=CIRCLE('',#9140,0.6);
#3517=CIRCLE('',#9142,0.33);
#3518=CIRCLE('',#9144,0.6);
#3519=CIRCLE('',#9145,0.6);
#3520=CIRCLE('',#9147,0.33);
#3521=CIRCLE('',#9149,0.6);
#3522=CIRCLE('',#9150,0.6);
#3523=CIRCLE('',#9152,0.33);
#3524=CIRCLE('',#9154,0.6);
#3525=CIRCLE('',#9155,0.6);
#3526=CIRCLE('',#9157,0.33);
#3527=CIRCLE('',#9159,4.);
#3528=CIRCLE('',#9160,4.);
#3529=CIRCLE('',#9161,4.);
#3530=CIRCLE('',#9162,4.);
#3531=CIRCLE('',#9163,2.6);
#3532=CIRCLE('',#9165,0.33);
#3533=CIRCLE('',#9167,0.33);
#3534=CIRCLE('',#9169,0.33);
#3535=CIRCLE('',#9171,0.33);
#3536=CIRCLE('',#9173,2.6);
#3537=CIRCLE('',#9175,2.2);
#3538=CIRCLE('',#9176,2.2);
#3539=CIRCLE('',#9178,4.);
#3540=CIRCLE('',#9183,0.225);
#3541=CIRCLE('',#9184,0.225);
#3542=CIRCLE('',#9186,0.225);
#3543=CIRCLE('',#9187,0.225);
#3544=CIRCLE('',#9189,0.225);
#3545=CIRCLE('',#9190,0.225);
#3546=CIRCLE('',#9192,0.225);
#3547=CIRCLE('',#9193,0.225);
#3548=CIRCLE('',#9195,2.59);
#3549=CIRCLE('',#9196,2.59);
#3550=CIRCLE('',#9198,2.);
#3551=CIRCLE('',#9200,2.);
#3552=CIRCLE('',#9202,4.);
#3553=CIRCLE('',#9203,4.);
#3554=CIRCLE('',#9216,0.2942);
#3555=CIRCLE('',#9218,0.45);
#3556=CIRCLE('',#9220,0.5);
#3557=CIRCLE('',#9222,0.5);
#3558=CIRCLE('',#9224,0.47);
#3559=CIRCLE('',#9226,0.32);
#3560=CIRCLE('',#9228,0.2942);
#3561=CIRCLE('',#9233,1.88531);
#3562=CIRCLE('',#9234,1.88531);
#3563=CIRCLE('',#9235,0.412776);
#3564=CIRCLE('',#9236,1.88531);
#3565=CIRCLE('',#9237,1.88531);
#3566=CIRCLE('',#9239,1.88531);
#3567=CIRCLE('',#9241,1.25);
#3568=CIRCLE('',#9242,1.25);
#3569=CIRCLE('',#9244,1.35);
#3570=CIRCLE('',#9247,1.88531);
#3571=CIRCLE('',#9249,1.35);
#3572=CIRCLE('',#9253,1.96469);
#3573=CIRCLE('',#9254,1.96469);
#3574=CIRCLE('',#9255,0.412776);
#3575=CIRCLE('',#9256,1.96469);
#3576=CIRCLE('',#9257,1.96469);
#3577=CIRCLE('',#9259,1.96469);
#3578=CIRCLE('',#9261,2.5);
#3579=CIRCLE('',#9262,1.96469);
#3580=CIRCLE('',#9264,2.6);
#3581=CIRCLE('',#9266,2.6);
#3582=CIRCLE('',#9268,2.5);
#3583=CIRCLE('',#9273,0.3969);
#3584=CIRCLE('',#9275,0.3969);
#3585=CIRCLE('',#9277,0.3969);
#3586=CIRCLE('',#9279,0.3969);
#3587=CIRCLE('',#9281,0.3969);
#3588=CIRCLE('',#9283,0.3969);
#3589=CIRCLE('',#9285,0.3969);
#3590=CIRCLE('',#9287,0.3969);
#3591=CIRCLE('',#9289,0.3969);
#3592=CIRCLE('',#9292,0.405071403305639);
#3593=CIRCLE('',#9293,0.405071403305639);
#3594=CIRCLE('',#9295,1.956752);
#3595=CIRCLE('',#9296,1.956752);
#3596=CIRCLE('',#9297,1.956752);
#3597=CIRCLE('',#9298,1.956752);
#3598=CIRCLE('',#9299,1.956752);
#3599=CIRCLE('',#9300,1.956752);
#3600=CIRCLE('',#9301,1.956752);
#3601=CIRCLE('',#9302,1.956752);
#3602=CIRCLE('',#9303,1.956752);
#3603=CIRCLE('',#9304,1.956752);
#3604=CIRCLE('',#9305,1.956752);
#3605=CIRCLE('',#9307,1.893248);
#3606=CIRCLE('',#9308,0.405071403305639);
#3607=CIRCLE('',#9310,0.405071403305639);
#3608=CIRCLE('',#9312,1.893248);
#3609=CIRCLE('',#9313,0.405071403305639);
#3610=CIRCLE('',#9315,0.405071403305639);
#3611=CIRCLE('',#9317,1.893248);
#3612=CIRCLE('',#9318,0.405071403305639);
#3613=CIRCLE('',#9320,0.405071403305639);
#3614=CIRCLE('',#9322,1.893248);
#3615=CIRCLE('',#9323,1.893248);
#3616=CIRCLE('',#9324,0.405071403305639);
#3617=CIRCLE('',#9326,0.405071403305639);
#3618=CIRCLE('',#9328,1.893248);
#3619=CIRCLE('',#9329,0.405071403305639);
#3620=CIRCLE('',#9331,0.405071403305639);
#3621=CIRCLE('',#9333,1.893248);
#3622=CIRCLE('',#9334,0.405071403305639);
#3623=CIRCLE('',#9336,0.405071403305639);
#3624=CIRCLE('',#9338,1.893248);
#3625=CIRCLE('',#9339,0.405071403305639);
#3626=CIRCLE('',#9341,0.405071403305639);
#3627=CIRCLE('',#9343,1.893248);
#3628=CIRCLE('',#9344,1.893248);
#3629=CIRCLE('',#9345,1.893248);
#3630=CIRCLE('',#9347,0.405071403305639);
#3631=CIRCLE('',#9349,0.405071403305639);
#3632=CIRCLE('',#9354,1.95469);
#3633=CIRCLE('',#9355,1.90031);
#3634=CIRCLE('',#9357,1.95469);
#3635=CIRCLE('',#9359,1.90031);
#3636=CIRCLE('',#9362,1.95469);
#3637=CIRCLE('',#9363,1.90031);
#3638=CIRCLE('',#9365,1.95469);
#3639=CIRCLE('',#9367,1.90031);
#3640=CIRCLE('',#9391,0.165);
#3641=CIRCLE('',#9392,0.165);
#3642=CIRCLE('',#9395,0.165);
#3643=CIRCLE('',#9396,0.165);
#3644=CIRCLE('',#9399,0.165);
#3645=CIRCLE('',#9400,0.165);
#3646=CIRCLE('',#9403,1.75);
#3647=CIRCLE('',#9404,1.25);
#3648=CIRCLE('',#9406,1.75);
#3649=CIRCLE('',#9408,1.25);
#3650=CIRCLE('',#9413,0.225);
#3651=CIRCLE('',#9414,0.225);
#3652=CIRCLE('',#9416,0.225);
#3653=CIRCLE('',#9417,0.225);
#3654=CIRCLE('',#9419,0.225);
#3655=CIRCLE('',#9420,0.225);
#3656=CIRCLE('',#9422,0.25);
#3657=CIRCLE('',#9423,0.25);
#3658=CIRCLE('',#9425,0.25);
#3659=CIRCLE('',#9426,0.25);
#3660=CIRCLE('',#9428,0.25);
#3661=CIRCLE('',#9429,0.25);
#3662=CIRCLE('',#9431,0.25);
#3663=CIRCLE('',#9432,0.25);
#3664=CIRCLE('',#9434,0.25);
#3665=CIRCLE('',#9435,0.25);
#3666=CIRCLE('',#9437,0.25);
#3667=CIRCLE('',#9438,0.25);
#3668=CIRCLE('',#9440,0.25);
#3669=CIRCLE('',#9441,0.25);
#3670=CIRCLE('',#9443,0.25);
#3671=CIRCLE('',#9444,0.25);
#3672=CIRCLE('',#9446,0.25);
#3673=CIRCLE('',#9447,0.25);
#3674=CIRCLE('',#9449,20.);
#3675=CIRCLE('',#9450,20.);
#3676=CIRCLE('',#9455,0.21);
#3677=CIRCLE('',#9456,0.21);
#3678=CIRCLE('',#9458,0.21);
#3679=CIRCLE('',#9461,1.255);
#3680=CIRCLE('',#9462,1.255);
#3681=CIRCLE('',#9464,1.8);
#3682=CIRCLE('',#9465,1.8);
#3683=CIRCLE('',#9470,0.3);
#3684=CIRCLE('',#9472,0.35);
#3685=CIRCLE('',#9474,0.35);
#3686=CIRCLE('',#9476,0.32);
#3687=CIRCLE('',#9478,0.22);
#3688=CIRCLE('',#9480,0.1954);
#3689=CIRCLE('',#9482,0.1954);
#3690=CIRCLE('',#9484,0.16);
#3691=CIRCLE('',#9517,0.22);
#3692=CIRCLE('',#9519,0.24505);
#3693=CIRCLE('',#9521,0.24505);
#3694=CIRCLE('',#9523,0.175);
#3695=CIRCLE('',#9535,0.275);
#3696=CIRCLE('',#9536,0.275);
#3697=CIRCLE('',#9538,0.275);
#3698=CIRCLE('',#9539,0.275);
#3699=CIRCLE('',#9541,0.275);
#3700=CIRCLE('',#9542,0.275);
#3701=CIRCLE('',#9544,0.275);
#3702=CIRCLE('',#9545,0.275);
#3703=CIRCLE('',#9547,0.5);
#3704=CIRCLE('',#9548,0.5);
#3705=CIRCLE('',#9550,0.5);
#3706=CIRCLE('',#9551,0.5);
#3707=CIRCLE('',#9570,0.165);
#3708=CIRCLE('',#9571,0.165);
#3709=CIRCLE('',#9574,0.8);
#3710=CIRCLE('',#9575,0.5);
#3711=CIRCLE('',#9577,0.8);
#3712=CIRCLE('',#9580,0.5);
#3713=CIRCLE('',#9584,0.505);
#3714=CIRCLE('',#9585,0.505);
#3715=CIRCLE('',#9587,0.7);
#3716=CIRCLE('',#9588,0.7);
#3717=CIRCLE('',#9593,0.505);
#3718=CIRCLE('',#9594,0.505);
#3719=CIRCLE('',#9596,0.7);
#3720=CIRCLE('',#9597,0.7);
#3721=CIRCLE('',#9602,0.225);
#3722=CIRCLE('',#9603,0.225);
#3723=CIRCLE('',#9605,0.8);
#3724=CIRCLE('',#9606,0.8);
#3725=CIRCLE('',#9612,0.275);
#3726=CIRCLE('',#9613,0.275);
#3727=CIRCLE('',#9615,0.275);
#3728=CIRCLE('',#9616,0.275);
#3729=CIRCLE('',#9618,0.275);
#3730=CIRCLE('',#9619,0.275);
#3731=CIRCLE('',#9621,0.275);
#3732=CIRCLE('',#9622,0.275);
#3733=CIRCLE('',#9624,0.5);
#3734=CIRCLE('',#9625,0.5);
#3735=CIRCLE('',#9627,0.5);
#3736=CIRCLE('',#9628,0.5);
#3737=CIRCLE('',#9647,0.165);
#3738=CIRCLE('',#9648,0.165);
#3739=CIRCLE('',#9651,0.8);
#3740=CIRCLE('',#9652,0.5);
#3741=CIRCLE('',#9654,0.8);
#3742=CIRCLE('',#9657,0.5);
#3743=CIRCLE('',#9661,0.505);
#3744=CIRCLE('',#9662,0.505);
#3745=CIRCLE('',#9664,0.7);
#3746=CIRCLE('',#9665,0.7);
#3747=CIRCLE('',#9670,0.505);
#3748=CIRCLE('',#9671,0.505);
#3749=CIRCLE('',#9673,0.7);
#3750=CIRCLE('',#9674,0.7);
#3751=CIRCLE('',#9679,0.225);
#3752=CIRCLE('',#9680,0.225);
#3753=CIRCLE('',#9682,0.8);
#3754=CIRCLE('',#9683,0.8);
#3755=CIRCLE('',#9689,0.275);
#3756=CIRCLE('',#9690,0.275);
#3757=CIRCLE('',#9692,0.275);
#3758=CIRCLE('',#9693,0.275);
#3759=CIRCLE('',#9695,0.275);
#3760=CIRCLE('',#9696,0.275);
#3761=CIRCLE('',#9698,0.275);
#3762=CIRCLE('',#9699,0.275);
#3763=CIRCLE('',#9701,0.5);
#3764=CIRCLE('',#9702,0.5);
#3765=CIRCLE('',#9704,0.5);
#3766=CIRCLE('',#9705,0.5);
#3767=CIRCLE('',#9724,0.165);
#3768=CIRCLE('',#9725,0.165);
#3769=CIRCLE('',#9728,0.8);
#3770=CIRCLE('',#9729,0.5);
#3771=CIRCLE('',#9731,0.8);
#3772=CIRCLE('',#9734,0.5);
#3773=CIRCLE('',#9738,0.505);
#3774=CIRCLE('',#9739,0.505);
#3775=CIRCLE('',#9741,0.7);
#3776=CIRCLE('',#9742,0.7);
#3777=CIRCLE('',#9747,0.505);
#3778=CIRCLE('',#9748,0.505);
#3779=CIRCLE('',#9750,0.7);
#3780=CIRCLE('',#9751,0.7);
#3781=CIRCLE('',#9756,0.225);
#3782=CIRCLE('',#9757,0.225);
#3783=CIRCLE('',#9759,0.8);
#3784=CIRCLE('',#9760,0.8);
#3785=CIRCLE('',#9766,0.275);
#3786=CIRCLE('',#9767,0.275);
#3787=CIRCLE('',#9769,0.275);
#3788=CIRCLE('',#9770,0.275);
#3789=CIRCLE('',#9772,0.275);
#3790=CIRCLE('',#9773,0.275);
#3791=CIRCLE('',#9775,0.275);
#3792=CIRCLE('',#9776,0.275);
#3793=CIRCLE('',#9778,0.5);
#3794=CIRCLE('',#9779,0.5);
#3795=CIRCLE('',#9781,0.5);
#3796=CIRCLE('',#9782,0.5);
#3797=CIRCLE('',#9801,0.165);
#3798=CIRCLE('',#9802,0.165);
#3799=CIRCLE('',#9805,0.8);
#3800=CIRCLE('',#9806,0.5);
#3801=CIRCLE('',#9808,0.8);
#3802=CIRCLE('',#9811,0.5);
#3803=CIRCLE('',#9815,0.505);
#3804=CIRCLE('',#9816,0.505);
#3805=CIRCLE('',#9818,0.7);
#3806=CIRCLE('',#9819,0.7);
#3807=CIRCLE('',#9824,0.505);
#3808=CIRCLE('',#9825,0.505);
#3809=CIRCLE('',#9827,0.7);
#3810=CIRCLE('',#9828,0.7);
#3811=CIRCLE('',#9833,0.225);
#3812=CIRCLE('',#9834,0.225);
#3813=CIRCLE('',#9836,0.8);
#3814=CIRCLE('',#9837,0.8);
#3815=CIRCLE('',#9850,0.24505);
#3816=CIRCLE('',#9852,0.375);
#3817=CIRCLE('',#9854,0.425);
#3818=CIRCLE('',#9856,0.425);
#3819=CIRCLE('',#9858,0.395);
#3820=CIRCLE('',#9860,0.27);
#3821=CIRCLE('',#9862,0.24505);
#3822=CIRCLE('',#9874,0.1954);
#3823=CIRCLE('',#9876,0.3);
#3824=CIRCLE('',#9878,0.35);
#3825=CIRCLE('',#9880,0.35);
#3826=CIRCLE('',#9882,0.32);
#3827=CIRCLE('',#9884,0.22);
#3828=CIRCLE('',#9886,0.1954);
#3829=CIRCLE('',#9931,1.5);
#3830=CIRCLE('',#9932,1.5);
#3831=CIRCLE('',#9934,2.);
#3832=CIRCLE('',#9935,2.);
#3833=CIRCLE('',#9940,1.1);
#3834=CIRCLE('',#9941,1.1);
#3835=CIRCLE('',#9943,1.5);
#3836=CIRCLE('',#9944,1.5);
#3837=CIRCLE('',#9949,1.1);
#3838=CIRCLE('',#9950,1.1);
#3839=CIRCLE('',#9952,1.5);
#3840=CIRCLE('',#9953,1.5);
#3841=CIRCLE('',#9959,1.5);
#3842=CIRCLE('',#9960,1.5);
#3843=CIRCLE('',#9962,2.);
#3844=CIRCLE('',#9963,2.);
#3845=CIRCLE('',#9968,1.1);
#3846=CIRCLE('',#9969,1.1);
#3847=CIRCLE('',#9971,1.5);
#3848=CIRCLE('',#9972,1.5);
#3849=CIRCLE('',#9977,1.1);
#3850=CIRCLE('',#9978,1.1);
#3851=CIRCLE('',#9980,1.5);
#3852=CIRCLE('',#9981,1.5);
#3853=CIRCLE('',#9987,1.5);
#3854=CIRCLE('',#9988,1.5);
#3855=CIRCLE('',#9990,2.);
#3856=CIRCLE('',#9991,2.);
#3857=CIRCLE('',#9996,1.1);
#3858=CIRCLE('',#9997,1.1);
#3859=CIRCLE('',#9999,1.5);
#3860=CIRCLE('',#10000,1.5);
#3861=CIRCLE('',#10005,1.1);
#3862=CIRCLE('',#10006,1.1);
#3863=CIRCLE('',#10008,1.5);
#3864=CIRCLE('',#10009,1.5);
#3865=CIRCLE('',#10015,1.5);
#3866=CIRCLE('',#10016,1.5);
#3867=CIRCLE('',#10018,2.);
#3868=CIRCLE('',#10019,2.);
#3869=CIRCLE('',#10024,1.1);
#3870=CIRCLE('',#10025,1.1);
#3871=CIRCLE('',#10027,1.5);
#3872=CIRCLE('',#10028,1.5);
#3873=CIRCLE('',#10033,1.1);
#3874=CIRCLE('',#10034,1.1);
#3875=CIRCLE('',#10036,1.5);
#3876=CIRCLE('',#10037,1.5);
#3877=CIRCLE('',#10043,0.976185);
#3878=CIRCLE('',#10044,0.976185);
#3879=CIRCLE('',#10045,0.247676);
#3880=CIRCLE('',#10046,0.976185);
#3881=CIRCLE('',#10047,0.976185);
#3882=CIRCLE('',#10049,0.976185);
#3883=CIRCLE('',#10051,0.5);
#3884=CIRCLE('',#10052,0.5);
#3885=CIRCLE('',#10054,0.56);
#3886=CIRCLE('',#10057,0.976185);
#3887=CIRCLE('',#10059,0.56);
#3888=CIRCLE('',#10063,1.023815);
#3889=CIRCLE('',#10064,1.023815);
#3890=CIRCLE('',#10065,0.247676);
#3891=CIRCLE('',#10066,1.023815);
#3892=CIRCLE('',#10067,1.023815);
#3893=CIRCLE('',#10069,1.023815);
#3894=CIRCLE('',#10071,1.44);
#3895=CIRCLE('',#10072,1.023815);
#3896=CIRCLE('',#10074,1.5);
#3897=CIRCLE('',#10076,1.5);
#3898=CIRCLE('',#10078,1.44);
#3899=CIRCLE('',#10083,0.23815);
#3900=CIRCLE('',#10085,0.23815);
#3901=CIRCLE('',#10087,0.23815);
#3902=CIRCLE('',#10089,0.23815);
#3903=CIRCLE('',#10091,0.23815);
#3904=CIRCLE('',#10093,0.23815);
#3905=CIRCLE('',#10095,0.23815);
#3906=CIRCLE('',#10097,0.23815);
#3907=CIRCLE('',#10100,0.243053047864041);
#3908=CIRCLE('',#10101,0.243053047864041);
#3909=CIRCLE('',#10103,1.019052);
#3910=CIRCLE('',#10104,1.019052);
#3911=CIRCLE('',#10105,1.019052);
#3912=CIRCLE('',#10106,1.019052);
#3913=CIRCLE('',#10107,1.019052);
#3914=CIRCLE('',#10108,1.019052);
#3915=CIRCLE('',#10109,1.019052);
#3916=CIRCLE('',#10110,1.019052);
#3917=CIRCLE('',#10111,1.019052);
#3918=CIRCLE('',#10113,0.980948);
#3919=CIRCLE('',#10114,0.243053047864041);
#3920=CIRCLE('',#10116,0.243053047864041);
#3921=CIRCLE('',#10118,0.980948);
#3922=CIRCLE('',#10119,0.243053047864041);
#3923=CIRCLE('',#10121,0.243053047864041);
#3924=CIRCLE('',#10123,0.980948);
#3925=CIRCLE('',#10124,0.243053047864041);
#3926=CIRCLE('',#10126,0.243053047864041);
#3927=CIRCLE('',#10128,0.980948);
#3928=CIRCLE('',#10129,0.243053047864041);
#3929=CIRCLE('',#10131,0.243053047864041);
#3930=CIRCLE('',#10133,0.980948);
#3931=CIRCLE('',#10134,0.243053047864041);
#3932=CIRCLE('',#10136,0.243053047864041);
#3933=CIRCLE('',#10138,0.980948);
#3934=CIRCLE('',#10139,0.243053047864041);
#3935=CIRCLE('',#10141,0.243053047864041);
#3936=CIRCLE('',#10143,0.980948);
#3937=CIRCLE('',#10144,0.980948);
#3938=CIRCLE('',#10145,0.980948);
#3939=CIRCLE('',#10147,0.243053047864041);
#3940=CIRCLE('',#10149,0.243053047864041);
#3941=CIRCLE('',#10154,1.013815);
#3942=CIRCLE('',#10155,0.991185);
#3943=CIRCLE('',#10157,1.013815);
#3944=CIRCLE('',#10159,0.991185);
#3945=CIRCLE('',#10162,1.013815);
#3946=CIRCLE('',#10163,0.991185);
#3947=CIRCLE('',#10165,1.013815);
#3948=CIRCLE('',#10167,0.991185);
#3949=VERTEX_POINT('',#13007);
#3950=VERTEX_POINT('',#13009);
#3951=VERTEX_POINT('',#13013);
#3952=VERTEX_POINT('',#13015);
#3953=VERTEX_POINT('',#13019);
#3954=VERTEX_POINT('',#13021);
#3955=VERTEX_POINT('',#13025);
#3956=VERTEX_POINT('',#13027);
#3957=VERTEX_POINT('',#13031);
#3958=VERTEX_POINT('',#13033);
#3959=VERTEX_POINT('',#13037);
#3960=VERTEX_POINT('',#13039);
#3961=VERTEX_POINT('',#13043);
#3962=VERTEX_POINT('',#13045);
#3963=VERTEX_POINT('',#13049);
#3964=VERTEX_POINT('',#13051);
#3965=VERTEX_POINT('',#13055);
#3966=VERTEX_POINT('',#13057);
#3967=VERTEX_POINT('',#13061);
#3968=VERTEX_POINT('',#13063);
#3969=VERTEX_POINT('',#13067);
#3970=VERTEX_POINT('',#13069);
#3971=VERTEX_POINT('',#13073);
#3972=VERTEX_POINT('',#13075);
#3973=VERTEX_POINT('',#13079);
#3974=VERTEX_POINT('',#13081);
#3975=VERTEX_POINT('',#13085);
#3976=VERTEX_POINT('',#13087);
#3977=VERTEX_POINT('',#13091);
#3978=VERTEX_POINT('',#13093);
#3979=VERTEX_POINT('',#13097);
#3980=VERTEX_POINT('',#13099);
#3981=VERTEX_POINT('',#13103);
#3982=VERTEX_POINT('',#13105);
#3983=VERTEX_POINT('',#13109);
#3984=VERTEX_POINT('',#13111);
#3985=VERTEX_POINT('',#13115);
#3986=VERTEX_POINT('',#13117);
#3987=VERTEX_POINT('',#13121);
#3988=VERTEX_POINT('',#13123);
#3989=VERTEX_POINT('',#13127);
#3990=VERTEX_POINT('',#13128);
#3991=VERTEX_POINT('',#13130);
#3992=VERTEX_POINT('',#13132);
#3993=VERTEX_POINT('',#13136);
#3994=VERTEX_POINT('',#13138);
#3995=VERTEX_POINT('',#13142);
#3996=VERTEX_POINT('',#13144);
#3997=VERTEX_POINT('',#13154);
#3998=VERTEX_POINT('',#13155);
#3999=VERTEX_POINT('',#13157);
#4000=VERTEX_POINT('',#13159);
#4001=VERTEX_POINT('',#13163);
#4002=VERTEX_POINT('',#13164);
#4003=VERTEX_POINT('',#13166);
#4004=VERTEX_POINT('',#13168);
#4005=VERTEX_POINT('',#13172);
#4006=VERTEX_POINT('',#13173);
#4007=VERTEX_POINT('',#13175);
#4008=VERTEX_POINT('',#13177);
#4009=VERTEX_POINT('',#13181);
#4010=VERTEX_POINT('',#13182);
#4011=VERTEX_POINT('',#13184);
#4012=VERTEX_POINT('',#13186);
#4013=VERTEX_POINT('',#13190);
#4014=VERTEX_POINT('',#13192);
#4015=VERTEX_POINT('',#13197);
#4016=VERTEX_POINT('',#13199);
#4017=VERTEX_POINT('',#13204);
#4018=VERTEX_POINT('',#13206);
#4019=VERTEX_POINT('',#13211);
#4020=VERTEX_POINT('',#13213);
#4021=VERTEX_POINT('',#13222);
#4022=VERTEX_POINT('',#13229);
#4023=VERTEX_POINT('',#13236);
#4024=VERTEX_POINT('',#13243);
#4025=VERTEX_POINT('',#13250);
#4026=VERTEX_POINT('',#13253);
#4027=VERTEX_POINT('',#13257);
#4028=VERTEX_POINT('',#13261);
#4029=VERTEX_POINT('',#13265);
#4030=VERTEX_POINT('',#13269);
#4031=VERTEX_POINT('',#13273);
#4032=VERTEX_POINT('',#13275);
#4033=VERTEX_POINT('',#13279);
#4034=VERTEX_POINT('',#13286);
#4035=VERTEX_POINT('',#13288);
#4036=VERTEX_POINT('',#13292);
#4037=VERTEX_POINT('',#13294);
#4038=VERTEX_POINT('',#13298);
#4039=VERTEX_POINT('',#13300);
#4040=VERTEX_POINT('',#13304);
#4041=VERTEX_POINT('',#13306);
#4042=VERTEX_POINT('',#13310);
#4043=VERTEX_POINT('',#13312);
#4044=VERTEX_POINT('',#13316);
#4045=VERTEX_POINT('',#13319);
#4046=VERTEX_POINT('',#13323);
#4047=VERTEX_POINT('',#13325);
#4048=VERTEX_POINT('',#13332);
#4049=VERTEX_POINT('',#13333);
#4050=VERTEX_POINT('',#13335);
#4051=VERTEX_POINT('',#13337);
#4052=VERTEX_POINT('',#13341);
#4053=VERTEX_POINT('',#13343);
#4054=VERTEX_POINT('',#13347);
#4055=VERTEX_POINT('',#13349);
#4056=VERTEX_POINT('',#13353);
#4057=VERTEX_POINT('',#13355);
#4058=VERTEX_POINT('',#13359);
#4059=VERTEX_POINT('',#13361);
#4060=VERTEX_POINT('',#13370);
#4061=VERTEX_POINT('',#13373);
#4062=VERTEX_POINT('',#13376);
#4063=VERTEX_POINT('',#13380);
#4064=VERTEX_POINT('',#13384);
#4065=VERTEX_POINT('',#13388);
#4066=VERTEX_POINT('',#13391);
#4067=VERTEX_POINT('',#13399);
#4068=VERTEX_POINT('',#13400);
#4069=VERTEX_POINT('',#13403);
#4070=VERTEX_POINT('',#13405);
#4071=VERTEX_POINT('',#13409);
#4072=VERTEX_POINT('',#13413);
#4073=VERTEX_POINT('',#13415);
#4074=VERTEX_POINT('',#13419);
#4075=VERTEX_POINT('',#13424);
#4076=VERTEX_POINT('',#13428);
#4077=VERTEX_POINT('',#13434);
#4078=VERTEX_POINT('',#13435);
#4079=VERTEX_POINT('',#13438);
#4080=VERTEX_POINT('',#13440);
#4081=VERTEX_POINT('',#13444);
#4082=VERTEX_POINT('',#13448);
#4083=VERTEX_POINT('',#13450);
#4084=VERTEX_POINT('',#13453);
#4085=VERTEX_POINT('',#13457);
#4086=VERTEX_POINT('',#13461);
#4087=VERTEX_POINT('',#13469);
#4088=VERTEX_POINT('',#13470);
#4089=VERTEX_POINT('',#13473);
#4090=VERTEX_POINT('',#13474);
#4091=VERTEX_POINT('',#13477);
#4092=VERTEX_POINT('',#13478);
#4093=VERTEX_POINT('',#13481);
#4094=VERTEX_POINT('',#13482);
#4095=VERTEX_POINT('',#13485);
#4096=VERTEX_POINT('',#13486);
#4097=VERTEX_POINT('',#13489);
#4098=VERTEX_POINT('',#13490);
#4099=VERTEX_POINT('',#13493);
#4100=VERTEX_POINT('',#13494);
#4101=VERTEX_POINT('',#13497);
#4102=VERTEX_POINT('',#13498);
#4103=VERTEX_POINT('',#13501);
#4104=VERTEX_POINT('',#13502);
#4105=VERTEX_POINT('',#13506);
#4106=VERTEX_POINT('',#13507);
#4107=VERTEX_POINT('',#13530);
#4108=VERTEX_POINT('',#13532);
#4109=VERTEX_POINT('',#13557);
#4110=VERTEX_POINT('',#13559);
#4111=VERTEX_POINT('',#13582);
#4112=VERTEX_POINT('',#13584);
#4113=VERTEX_POINT('',#13607);
#4114=VERTEX_POINT('',#13609);
#4115=VERTEX_POINT('',#13632);
#4116=VERTEX_POINT('',#13634);
#4117=VERTEX_POINT('',#13637);
#4118=VERTEX_POINT('',#13639);
#4119=VERTEX_POINT('',#13662);
#4120=VERTEX_POINT('',#13664);
#4121=VERTEX_POINT('',#13687);
#4122=VERTEX_POINT('',#13689);
#4123=VERTEX_POINT('',#13712);
#4124=VERTEX_POINT('',#13714);
#4125=VERTEX_POINT('',#13737);
#4126=VERTEX_POINT('',#13739);
#4127=VERTEX_POINT('',#13764);
#4128=VERTEX_POINT('',#13768);
#4129=VERTEX_POINT('',#13793);
#4130=VERTEX_POINT('',#13797);
#4131=VERTEX_POINT('',#13822);
#4132=VERTEX_POINT('',#13826);
#4133=VERTEX_POINT('',#13851);
#4134=VERTEX_POINT('',#13853);
#4135=VERTEX_POINT('',#13857);
#4136=VERTEX_POINT('',#13882);
#4137=VERTEX_POINT('',#13886);
#4138=VERTEX_POINT('',#13911);
#4139=VERTEX_POINT('',#13915);
#4140=VERTEX_POINT('',#13940);
#4141=VERTEX_POINT('',#13944);
#4142=VERTEX_POINT('',#13969);
#4143=VERTEX_POINT('',#13972);
#4144=VERTEX_POINT('',#13974);
#4145=VERTEX_POINT('',#14006);
#4146=VERTEX_POINT('',#14008);
#4147=VERTEX_POINT('',#14011);
#4148=VERTEX_POINT('',#14015);
#4149=VERTEX_POINT('',#14020);
#4150=VERTEX_POINT('',#14022);
#4151=VERTEX_POINT('',#14025);
#4152=VERTEX_POINT('',#14029);
#4153=VERTEX_POINT('',#14040);
#4154=VERTEX_POINT('',#14041);
#4155=VERTEX_POINT('',#14043);
#4156=VERTEX_POINT('',#14045);
#4157=VERTEX_POINT('',#14049);
#4158=VERTEX_POINT('',#14051);
#4159=VERTEX_POINT('',#14055);
#4160=VERTEX_POINT('',#14057);
#4161=VERTEX_POINT('',#14067);
#4162=VERTEX_POINT('',#14068);
#4163=VERTEX_POINT('',#14070);
#4164=VERTEX_POINT('',#14072);
#4165=VERTEX_POINT('',#14076);
#4166=VERTEX_POINT('',#14078);
#4167=VERTEX_POINT('',#14082);
#4168=VERTEX_POINT('',#14084);
#4169=VERTEX_POINT('',#14095);
#4170=VERTEX_POINT('',#14097);
#4171=VERTEX_POINT('',#14102);
#4172=VERTEX_POINT('',#14104);
#4173=VERTEX_POINT('',#14109);
#4174=VERTEX_POINT('',#14111);
#4175=VERTEX_POINT('',#14116);
#4176=VERTEX_POINT('',#14118);
#4177=VERTEX_POINT('',#14121);
#4178=VERTEX_POINT('',#14125);
#4179=VERTEX_POINT('',#14132);
#4180=VERTEX_POINT('',#14134);
#4181=VERTEX_POINT('',#14138);
#4182=VERTEX_POINT('',#14140);
#4183=VERTEX_POINT('',#14144);
#4184=VERTEX_POINT('',#14146);
#4185=VERTEX_POINT('',#14150);
#4186=VERTEX_POINT('',#14152);
#4187=VERTEX_POINT('',#14156);
#4188=VERTEX_POINT('',#14158);
#4189=VERTEX_POINT('',#14162);
#4190=VERTEX_POINT('',#14164);
#4191=VERTEX_POINT('',#14168);
#4192=VERTEX_POINT('',#14170);
#4193=VERTEX_POINT('',#14174);
#4194=VERTEX_POINT('',#14176);
#4195=VERTEX_POINT('',#14180);
#4196=VERTEX_POINT('',#14182);
#4197=VERTEX_POINT('',#14186);
#4198=VERTEX_POINT('',#14188);
#4199=VERTEX_POINT('',#14192);
#4200=VERTEX_POINT('',#14194);
#4201=VERTEX_POINT('',#14198);
#4202=VERTEX_POINT('',#14200);
#4203=VERTEX_POINT('',#14204);
#4204=VERTEX_POINT('',#14206);
#4205=VERTEX_POINT('',#14213);
#4206=VERTEX_POINT('',#14214);
#4207=VERTEX_POINT('',#14216);
#4208=VERTEX_POINT('',#14220);
#4209=VERTEX_POINT('',#14235);
#4210=VERTEX_POINT('',#14251);
#4211=VERTEX_POINT('',#14290);
#4212=VERTEX_POINT('',#14292);
#4213=VERTEX_POINT('',#14296);
#4214=VERTEX_POINT('',#14298);
#4215=VERTEX_POINT('',#14305);
#4216=VERTEX_POINT('',#14308);
#4217=VERTEX_POINT('',#14312);
#4218=VERTEX_POINT('',#14316);
#4219=VERTEX_POINT('',#14320);
#4220=VERTEX_POINT('',#14323);
#4221=VERTEX_POINT('',#14327);
#4222=VERTEX_POINT('',#14331);
#4223=VERTEX_POINT('',#14336);
#4224=VERTEX_POINT('',#14337);
#4225=VERTEX_POINT('',#14339);
#4226=VERTEX_POINT('',#14341);
#4227=VERTEX_POINT('',#14345);
#4228=VERTEX_POINT('',#14347);
#4229=VERTEX_POINT('',#14351);
#4230=VERTEX_POINT('',#14353);
#4231=VERTEX_POINT('',#14357);
#4232=VERTEX_POINT('',#14359);
#4233=VERTEX_POINT('',#14363);
#4234=VERTEX_POINT('',#14365);
#4235=VERTEX_POINT('',#14389);
#4236=VERTEX_POINT('',#14390);
#4237=VERTEX_POINT('',#14392);
#4238=VERTEX_POINT('',#14394);
#4239=VERTEX_POINT('',#14398);
#4240=VERTEX_POINT('',#14400);
#4241=VERTEX_POINT('',#14404);
#4242=VERTEX_POINT('',#14406);
#4243=VERTEX_POINT('',#14410);
#4244=VERTEX_POINT('',#14412);
#4245=VERTEX_POINT('',#14416);
#4246=VERTEX_POINT('',#14418);
#4247=VERTEX_POINT('',#14426);
#4248=VERTEX_POINT('',#14429);
#4249=VERTEX_POINT('',#14433);
#4250=VERTEX_POINT('',#14437);
#4251=VERTEX_POINT('',#14451);
#4252=VERTEX_POINT('',#14453);
#4253=VERTEX_POINT('',#14457);
#4254=VERTEX_POINT('',#14459);
#4255=VERTEX_POINT('',#14463);
#4256=VERTEX_POINT('',#14465);
#4257=VERTEX_POINT('',#14469);
#4258=VERTEX_POINT('',#14471);
#4259=VERTEX_POINT('',#14475);
#4260=VERTEX_POINT('',#14477);
#4261=VERTEX_POINT('',#14481);
#4262=VERTEX_POINT('',#14483);
#4263=VERTEX_POINT('',#14487);
#4264=VERTEX_POINT('',#14488);
#4265=VERTEX_POINT('',#14490);
#4266=VERTEX_POINT('',#14492);
#4267=VERTEX_POINT('',#14496);
#4268=VERTEX_POINT('',#14497);
#4269=VERTEX_POINT('',#14499);
#4270=VERTEX_POINT('',#14501);
#4271=VERTEX_POINT('',#14512);
#4272=VERTEX_POINT('',#14513);
#4273=VERTEX_POINT('',#14515);
#4274=VERTEX_POINT('',#14517);
#4275=VERTEX_POINT('',#14521);
#4276=VERTEX_POINT('',#14522);
#4277=VERTEX_POINT('',#14524);
#4278=VERTEX_POINT('',#14526);
#4279=VERTEX_POINT('',#14537);
#4280=VERTEX_POINT('',#14538);
#4281=VERTEX_POINT('',#14540);
#4282=VERTEX_POINT('',#14542);
#4283=VERTEX_POINT('',#14546);
#4284=VERTEX_POINT('',#14548);
#4285=VERTEX_POINT('',#14552);
#4286=VERTEX_POINT('',#14554);
#4287=VERTEX_POINT('',#14564);
#4288=VERTEX_POINT('',#14566);
#4289=VERTEX_POINT('',#14571);
#4290=VERTEX_POINT('',#14573);
#4291=VERTEX_POINT('',#14576);
#4292=VERTEX_POINT('',#14581);
#4293=VERTEX_POINT('',#14587);
#4294=VERTEX_POINT('',#14589);
#4295=VERTEX_POINT('',#14593);
#4296=VERTEX_POINT('',#14595);
#4297=VERTEX_POINT('',#14602);
#4298=VERTEX_POINT('',#14604);
#4299=VERTEX_POINT('',#14608);
#4300=VERTEX_POINT('',#14610);
#4301=VERTEX_POINT('',#14617);
#4302=VERTEX_POINT('',#14619);
#4303=VERTEX_POINT('',#14623);
#4304=VERTEX_POINT('',#14625);
#4305=VERTEX_POINT('',#14633);
#4306=VERTEX_POINT('',#14635);
#4307=VERTEX_POINT('',#14639);
#4308=VERTEX_POINT('',#14641);
#4309=VERTEX_POINT('',#14645);
#4310=VERTEX_POINT('',#14647);
#4311=VERTEX_POINT('',#14651);
#4312=VERTEX_POINT('',#14653);
#4313=VERTEX_POINT('',#14657);
#4314=VERTEX_POINT('',#14659);
#4315=VERTEX_POINT('',#14663);
#4316=VERTEX_POINT('',#14665);
#4317=VERTEX_POINT('',#14669);
#4318=VERTEX_POINT('',#14670);
#4319=VERTEX_POINT('',#14672);
#4320=VERTEX_POINT('',#14674);
#4321=VERTEX_POINT('',#14678);
#4322=VERTEX_POINT('',#14679);
#4323=VERTEX_POINT('',#14681);
#4324=VERTEX_POINT('',#14683);
#4325=VERTEX_POINT('',#14694);
#4326=VERTEX_POINT('',#14695);
#4327=VERTEX_POINT('',#14697);
#4328=VERTEX_POINT('',#14699);
#4329=VERTEX_POINT('',#14703);
#4330=VERTEX_POINT('',#14704);
#4331=VERTEX_POINT('',#14706);
#4332=VERTEX_POINT('',#14708);
#4333=VERTEX_POINT('',#14719);
#4334=VERTEX_POINT('',#14720);
#4335=VERTEX_POINT('',#14722);
#4336=VERTEX_POINT('',#14724);
#4337=VERTEX_POINT('',#14728);
#4338=VERTEX_POINT('',#14730);
#4339=VERTEX_POINT('',#14734);
#4340=VERTEX_POINT('',#14736);
#4341=VERTEX_POINT('',#14746);
#4342=VERTEX_POINT('',#14748);
#4343=VERTEX_POINT('',#14753);
#4344=VERTEX_POINT('',#14755);
#4345=VERTEX_POINT('',#14758);
#4346=VERTEX_POINT('',#14763);
#4347=VERTEX_POINT('',#14769);
#4348=VERTEX_POINT('',#14771);
#4349=VERTEX_POINT('',#14775);
#4350=VERTEX_POINT('',#14777);
#4351=VERTEX_POINT('',#14784);
#4352=VERTEX_POINT('',#14786);
#4353=VERTEX_POINT('',#14790);
#4354=VERTEX_POINT('',#14792);
#4355=VERTEX_POINT('',#14799);
#4356=VERTEX_POINT('',#14801);
#4357=VERTEX_POINT('',#14805);
#4358=VERTEX_POINT('',#14807);
#4359=VERTEX_POINT('',#14815);
#4360=VERTEX_POINT('',#14817);
#4361=VERTEX_POINT('',#14821);
#4362=VERTEX_POINT('',#14823);
#4363=VERTEX_POINT('',#14827);
#4364=VERTEX_POINT('',#14829);
#4365=VERTEX_POINT('',#14833);
#4366=VERTEX_POINT('',#14835);
#4367=VERTEX_POINT('',#14839);
#4368=VERTEX_POINT('',#14841);
#4369=VERTEX_POINT('',#14845);
#4370=VERTEX_POINT('',#14847);
#4371=VERTEX_POINT('',#14851);
#4372=VERTEX_POINT('',#14852);
#4373=VERTEX_POINT('',#14854);
#4374=VERTEX_POINT('',#14856);
#4375=VERTEX_POINT('',#14860);
#4376=VERTEX_POINT('',#14861);
#4377=VERTEX_POINT('',#14863);
#4378=VERTEX_POINT('',#14865);
#4379=VERTEX_POINT('',#14876);
#4380=VERTEX_POINT('',#14877);
#4381=VERTEX_POINT('',#14879);
#4382=VERTEX_POINT('',#14881);
#4383=VERTEX_POINT('',#14885);
#4384=VERTEX_POINT('',#14886);
#4385=VERTEX_POINT('',#14888);
#4386=VERTEX_POINT('',#14890);
#4387=VERTEX_POINT('',#14901);
#4388=VERTEX_POINT('',#14902);
#4389=VERTEX_POINT('',#14904);
#4390=VERTEX_POINT('',#14906);
#4391=VERTEX_POINT('',#14910);
#4392=VERTEX_POINT('',#14912);
#4393=VERTEX_POINT('',#14916);
#4394=VERTEX_POINT('',#14918);
#4395=VERTEX_POINT('',#14928);
#4396=VERTEX_POINT('',#14930);
#4397=VERTEX_POINT('',#14935);
#4398=VERTEX_POINT('',#14937);
#4399=VERTEX_POINT('',#14940);
#4400=VERTEX_POINT('',#14945);
#4401=VERTEX_POINT('',#14951);
#4402=VERTEX_POINT('',#14953);
#4403=VERTEX_POINT('',#14957);
#4404=VERTEX_POINT('',#14959);
#4405=VERTEX_POINT('',#14966);
#4406=VERTEX_POINT('',#14968);
#4407=VERTEX_POINT('',#14972);
#4408=VERTEX_POINT('',#14974);
#4409=VERTEX_POINT('',#14981);
#4410=VERTEX_POINT('',#14983);
#4411=VERTEX_POINT('',#14987);
#4412=VERTEX_POINT('',#14989);
#4413=VERTEX_POINT('',#14997);
#4414=VERTEX_POINT('',#14999);
#4415=VERTEX_POINT('',#15003);
#4416=VERTEX_POINT('',#15005);
#4417=VERTEX_POINT('',#15009);
#4418=VERTEX_POINT('',#15011);
#4419=VERTEX_POINT('',#15015);
#4420=VERTEX_POINT('',#15017);
#4421=VERTEX_POINT('',#15021);
#4422=VERTEX_POINT('',#15023);
#4423=VERTEX_POINT('',#15027);
#4424=VERTEX_POINT('',#15029);
#4425=VERTEX_POINT('',#15033);
#4426=VERTEX_POINT('',#15034);
#4427=VERTEX_POINT('',#15036);
#4428=VERTEX_POINT('',#15038);
#4429=VERTEX_POINT('',#15042);
#4430=VERTEX_POINT('',#15043);
#4431=VERTEX_POINT('',#15045);
#4432=VERTEX_POINT('',#15047);
#4433=VERTEX_POINT('',#15058);
#4434=VERTEX_POINT('',#15059);
#4435=VERTEX_POINT('',#15061);
#4436=VERTEX_POINT('',#15063);
#4437=VERTEX_POINT('',#15067);
#4438=VERTEX_POINT('',#15068);
#4439=VERTEX_POINT('',#15070);
#4440=VERTEX_POINT('',#15072);
#4441=VERTEX_POINT('',#15083);
#4442=VERTEX_POINT('',#15084);
#4443=VERTEX_POINT('',#15086);
#4444=VERTEX_POINT('',#15088);
#4445=VERTEX_POINT('',#15092);
#4446=VERTEX_POINT('',#15094);
#4447=VERTEX_POINT('',#15098);
#4448=VERTEX_POINT('',#15100);
#4449=VERTEX_POINT('',#15110);
#4450=VERTEX_POINT('',#15112);
#4451=VERTEX_POINT('',#15117);
#4452=VERTEX_POINT('',#15119);
#4453=VERTEX_POINT('',#15122);
#4454=VERTEX_POINT('',#15127);
#4455=VERTEX_POINT('',#15133);
#4456=VERTEX_POINT('',#15135);
#4457=VERTEX_POINT('',#15139);
#4458=VERTEX_POINT('',#15141);
#4459=VERTEX_POINT('',#15148);
#4460=VERTEX_POINT('',#15150);
#4461=VERTEX_POINT('',#15154);
#4462=VERTEX_POINT('',#15156);
#4463=VERTEX_POINT('',#15163);
#4464=VERTEX_POINT('',#15165);
#4465=VERTEX_POINT('',#15169);
#4466=VERTEX_POINT('',#15171);
#4467=VERTEX_POINT('',#15178);
#4468=VERTEX_POINT('',#15179);
#4469=VERTEX_POINT('',#15181);
#4470=VERTEX_POINT('',#15183);
#4471=VERTEX_POINT('',#15187);
#4472=VERTEX_POINT('',#15189);
#4473=VERTEX_POINT('',#15193);
#4474=VERTEX_POINT('',#15195);
#4475=VERTEX_POINT('',#15199);
#4476=VERTEX_POINT('',#15201);
#4477=VERTEX_POINT('',#15205);
#4478=VERTEX_POINT('',#15207);
#4479=VERTEX_POINT('',#15216);
#4480=VERTEX_POINT('',#15219);
#4481=VERTEX_POINT('',#15222);
#4482=VERTEX_POINT('',#15226);
#4483=VERTEX_POINT('',#15230);
#4484=VERTEX_POINT('',#15234);
#4485=VERTEX_POINT('',#15237);
#4486=VERTEX_POINT('',#15244);
#4487=VERTEX_POINT('',#15245);
#4488=VERTEX_POINT('',#15247);
#4489=VERTEX_POINT('',#15249);
#4490=VERTEX_POINT('',#15253);
#4491=VERTEX_POINT('',#15255);
#4492=VERTEX_POINT('',#15259);
#4493=VERTEX_POINT('',#15261);
#4494=VERTEX_POINT('',#15265);
#4495=VERTEX_POINT('',#15267);
#4496=VERTEX_POINT('',#15271);
#4497=VERTEX_POINT('',#15273);
#4498=VERTEX_POINT('',#15282);
#4499=VERTEX_POINT('',#15285);
#4500=VERTEX_POINT('',#15288);
#4501=VERTEX_POINT('',#15292);
#4502=VERTEX_POINT('',#15296);
#4503=VERTEX_POINT('',#15300);
#4504=VERTEX_POINT('',#15303);
#4505=VERTEX_POINT('',#15351);
#4506=VERTEX_POINT('',#15353);
#4507=VERTEX_POINT('',#15357);
#4508=VERTEX_POINT('',#15359);
#4509=VERTEX_POINT('',#15366);
#4510=VERTEX_POINT('',#15368);
#4511=VERTEX_POINT('',#15372);
#4512=VERTEX_POINT('',#15374);
#4513=VERTEX_POINT('',#15381);
#4514=VERTEX_POINT('',#15383);
#4515=VERTEX_POINT('',#15387);
#4516=VERTEX_POINT('',#15389);
#4517=VERTEX_POINT('',#15397);
#4518=VERTEX_POINT('',#15399);
#4519=VERTEX_POINT('',#15403);
#4520=VERTEX_POINT('',#15405);
#4521=VERTEX_POINT('',#15412);
#4522=VERTEX_POINT('',#15414);
#4523=VERTEX_POINT('',#15418);
#4524=VERTEX_POINT('',#15420);
#4525=VERTEX_POINT('',#15427);
#4526=VERTEX_POINT('',#15429);
#4527=VERTEX_POINT('',#15433);
#4528=VERTEX_POINT('',#15435);
#4529=VERTEX_POINT('',#15443);
#4530=VERTEX_POINT('',#15445);
#4531=VERTEX_POINT('',#15449);
#4532=VERTEX_POINT('',#15451);
#4533=VERTEX_POINT('',#15458);
#4534=VERTEX_POINT('',#15460);
#4535=VERTEX_POINT('',#15464);
#4536=VERTEX_POINT('',#15466);
#4537=VERTEX_POINT('',#15473);
#4538=VERTEX_POINT('',#15475);
#4539=VERTEX_POINT('',#15479);
#4540=VERTEX_POINT('',#15481);
#4541=VERTEX_POINT('',#15489);
#4542=VERTEX_POINT('',#15491);
#4543=VERTEX_POINT('',#15495);
#4544=VERTEX_POINT('',#15497);
#4545=VERTEX_POINT('',#15504);
#4546=VERTEX_POINT('',#15506);
#4547=VERTEX_POINT('',#15510);
#4548=VERTEX_POINT('',#15512);
#4549=VERTEX_POINT('',#15519);
#4550=VERTEX_POINT('',#15521);
#4551=VERTEX_POINT('',#15525);
#4552=VERTEX_POINT('',#15527);
#4553=VERTEX_POINT('',#15535);
#4554=VERTEX_POINT('',#15536);
#4555=VERTEX_POINT('',#15539);
#4556=VERTEX_POINT('',#15541);
#4557=VERTEX_POINT('',#15545);
#4558=VERTEX_POINT('',#15549);
#4559=VERTEX_POINT('',#15551);
#4560=VERTEX_POINT('',#15555);
#4561=VERTEX_POINT('',#15560);
#4562=VERTEX_POINT('',#15564);
#4563=VERTEX_POINT('',#15570);
#4564=VERTEX_POINT('',#15571);
#4565=VERTEX_POINT('',#15574);
#4566=VERTEX_POINT('',#15576);
#4567=VERTEX_POINT('',#15580);
#4568=VERTEX_POINT('',#15584);
#4569=VERTEX_POINT('',#15586);
#4570=VERTEX_POINT('',#15589);
#4571=VERTEX_POINT('',#15593);
#4572=VERTEX_POINT('',#15597);
#4573=VERTEX_POINT('',#15605);
#4574=VERTEX_POINT('',#15606);
#4575=VERTEX_POINT('',#15609);
#4576=VERTEX_POINT('',#15610);
#4577=VERTEX_POINT('',#15613);
#4578=VERTEX_POINT('',#15614);
#4579=VERTEX_POINT('',#15617);
#4580=VERTEX_POINT('',#15618);
#4581=VERTEX_POINT('',#15621);
#4582=VERTEX_POINT('',#15622);
#4583=VERTEX_POINT('',#15625);
#4584=VERTEX_POINT('',#15626);
#4585=VERTEX_POINT('',#15629);
#4586=VERTEX_POINT('',#15630);
#4587=VERTEX_POINT('',#15633);
#4588=VERTEX_POINT('',#15634);
#4589=VERTEX_POINT('',#15638);
#4590=VERTEX_POINT('',#15639);
#4591=VERTEX_POINT('',#15662);
#4592=VERTEX_POINT('',#15664);
#4593=VERTEX_POINT('',#15689);
#4594=VERTEX_POINT('',#15691);
#4595=VERTEX_POINT('',#15714);
#4596=VERTEX_POINT('',#15716);
#4597=VERTEX_POINT('',#15739);
#4598=VERTEX_POINT('',#15741);
#4599=VERTEX_POINT('',#15754);
#4600=VERTEX_POINT('',#15757);
#4601=VERTEX_POINT('',#15770);
#4602=VERTEX_POINT('',#15772);
#4603=VERTEX_POINT('',#15795);
#4604=VERTEX_POINT('',#15797);
#4605=VERTEX_POINT('',#15820);
#4606=VERTEX_POINT('',#15822);
#4607=VERTEX_POINT('',#15845);
#4608=VERTEX_POINT('',#15847);
#4609=VERTEX_POINT('',#15872);
#4610=VERTEX_POINT('',#15876);
#4611=VERTEX_POINT('',#15901);
#4612=VERTEX_POINT('',#15905);
#4613=VERTEX_POINT('',#15930);
#4614=VERTEX_POINT('',#15934);
#4615=VERTEX_POINT('',#15935);
#4616=VERTEX_POINT('',#15962);
#4617=VERTEX_POINT('',#15966);
#4618=VERTEX_POINT('',#15991);
#4619=VERTEX_POINT('',#15995);
#4620=VERTEX_POINT('',#16020);
#4621=VERTEX_POINT('',#16024);
#4622=VERTEX_POINT('',#16049);
#4623=VERTEX_POINT('',#16052);
#4624=VERTEX_POINT('',#16054);
#4625=VERTEX_POINT('',#16086);
#4626=VERTEX_POINT('',#16088);
#4627=VERTEX_POINT('',#16091);
#4628=VERTEX_POINT('',#16095);
#4629=VERTEX_POINT('',#16100);
#4630=VERTEX_POINT('',#16102);
#4631=VERTEX_POINT('',#16105);
#4632=VERTEX_POINT('',#16109);
#4633=EDGE_CURVE('',#3949,#3949,#3459,.T.);
#4634=EDGE_CURVE('',#3949,#3950,#2493,.T.);
#4635=EDGE_CURVE('',#3950,#3950,#3460,.T.);
#4636=EDGE_CURVE('',#3951,#3951,#3461,.T.);
#4637=EDGE_CURVE('',#3951,#3952,#2494,.T.);
#4638=EDGE_CURVE('',#3952,#3952,#3462,.T.);
#4639=EDGE_CURVE('',#3953,#3953,#3463,.T.);
#4640=EDGE_CURVE('',#3953,#3954,#2495,.T.);
#4641=EDGE_CURVE('',#3954,#3954,#3464,.T.);
#4642=EDGE_CURVE('',#3955,#3955,#3465,.T.);
#4643=EDGE_CURVE('',#3955,#3956,#2496,.T.);
#4644=EDGE_CURVE('',#3956,#3956,#3466,.T.);
#4645=EDGE_CURVE('',#3957,#3957,#3467,.T.);
#4646=EDGE_CURVE('',#3957,#3958,#2497,.T.);
#4647=EDGE_CURVE('',#3958,#3958,#3468,.T.);
#4648=EDGE_CURVE('',#3959,#3959,#3469,.T.);
#4649=EDGE_CURVE('',#3959,#3960,#2498,.T.);
#4650=EDGE_CURVE('',#3960,#3960,#3470,.T.);
#4651=EDGE_CURVE('',#3961,#3961,#3471,.T.);
#4652=EDGE_CURVE('',#3961,#3962,#2499,.T.);
#4653=EDGE_CURVE('',#3962,#3962,#3472,.T.);
#4654=EDGE_CURVE('',#3963,#3963,#3473,.T.);
#4655=EDGE_CURVE('',#3963,#3964,#2500,.T.);
#4656=EDGE_CURVE('',#3964,#3964,#3474,.T.);
#4657=EDGE_CURVE('',#3965,#3965,#3475,.T.);
#4658=EDGE_CURVE('',#3965,#3966,#2501,.T.);
#4659=EDGE_CURVE('',#3966,#3966,#3476,.T.);
#4660=EDGE_CURVE('',#3967,#3967,#3477,.T.);
#4661=EDGE_CURVE('',#3967,#3968,#2502,.T.);
#4662=EDGE_CURVE('',#3968,#3968,#3478,.T.);
#4663=EDGE_CURVE('',#3969,#3969,#3479,.T.);
#4664=EDGE_CURVE('',#3969,#3970,#2503,.T.);
#4665=EDGE_CURVE('',#3970,#3970,#3480,.T.);
#4666=EDGE_CURVE('',#3971,#3971,#3481,.T.);
#4667=EDGE_CURVE('',#3971,#3972,#2504,.T.);
#4668=EDGE_CURVE('',#3972,#3972,#3482,.T.);
#4669=EDGE_CURVE('',#3973,#3973,#3483,.T.);
#4670=EDGE_CURVE('',#3973,#3974,#2505,.T.);
#4671=EDGE_CURVE('',#3974,#3974,#3484,.T.);
#4672=EDGE_CURVE('',#3975,#3975,#3485,.T.);
#4673=EDGE_CURVE('',#3975,#3976,#2506,.T.);
#4674=EDGE_CURVE('',#3976,#3976,#3486,.T.);
#4675=EDGE_CURVE('',#3977,#3977,#3487,.T.);
#4676=EDGE_CURVE('',#3977,#3978,#2507,.T.);
#4677=EDGE_CURVE('',#3978,#3978,#3488,.T.);
#4678=EDGE_CURVE('',#3979,#3979,#3489,.T.);
#4679=EDGE_CURVE('',#3979,#3980,#2508,.T.);
#4680=EDGE_CURVE('',#3980,#3980,#3490,.T.);
#4681=EDGE_CURVE('',#3981,#3981,#3491,.T.);
#4682=EDGE_CURVE('',#3981,#3982,#2509,.T.);
#4683=EDGE_CURVE('',#3982,#3982,#3492,.T.);
#4684=EDGE_CURVE('',#3983,#3983,#3493,.T.);
#4685=EDGE_CURVE('',#3983,#3984,#2510,.T.);
#4686=EDGE_CURVE('',#3984,#3984,#3494,.T.);
#4687=EDGE_CURVE('',#3985,#3985,#3495,.T.);
#4688=EDGE_CURVE('',#3985,#3986,#2511,.T.);
#4689=EDGE_CURVE('',#3986,#3986,#3496,.T.);
#4690=EDGE_CURVE('',#3987,#3987,#3497,.T.);
#4691=EDGE_CURVE('',#3987,#3988,#2512,.T.);
#4692=EDGE_CURVE('',#3988,#3988,#3498,.T.);
#4693=EDGE_CURVE('',#3989,#3990,#2513,.T.);
#4694=EDGE_CURVE('',#3990,#3991,#2514,.T.);
#4695=EDGE_CURVE('',#3992,#3991,#2515,.T.);
#4696=EDGE_CURVE('',#3989,#3992,#2516,.T.);
#4697=EDGE_CURVE('',#3993,#3989,#2517,.T.);
#4698=EDGE_CURVE('',#3994,#3992,#2518,.T.);
#4699=EDGE_CURVE('',#3993,#3994,#2519,.T.);
#4700=EDGE_CURVE('',#3995,#3993,#2520,.T.);
#4701=EDGE_CURVE('',#3996,#3994,#2521,.T.);
#4702=EDGE_CURVE('',#3995,#3996,#2522,.T.);
#4703=EDGE_CURVE('',#3990,#3995,#2523,.T.);
#4704=EDGE_CURVE('',#3991,#3996,#2524,.T.);
#4705=EDGE_CURVE('',#3997,#3998,#2525,.T.);
#4706=EDGE_CURVE('',#3999,#3997,#3499,.T.);
#4707=EDGE_CURVE('',#3999,#4000,#2526,.T.);
#4708=EDGE_CURVE('',#3998,#4000,#3500,.T.);
#4709=EDGE_CURVE('',#4001,#4002,#2527,.T.);
#4710=EDGE_CURVE('',#4003,#4001,#3501,.T.);
#4711=EDGE_CURVE('',#4003,#4004,#2528,.T.);
#4712=EDGE_CURVE('',#4002,#4004,#3502,.T.);
#4713=EDGE_CURVE('',#4005,#4006,#2529,.T.);
#4714=EDGE_CURVE('',#4007,#4005,#3503,.T.);
#4715=EDGE_CURVE('',#4007,#4008,#2530,.T.);
#4716=EDGE_CURVE('',#4006,#4008,#3504,.T.);
#4717=EDGE_CURVE('',#4009,#4010,#2531,.T.);
#4718=EDGE_CURVE('',#4011,#4009,#3505,.T.);
#4719=EDGE_CURVE('',#4011,#4012,#2532,.T.);
#4720=EDGE_CURVE('',#4010,#4012,#3506,.T.);
#4721=EDGE_CURVE('',#4013,#4013,#3507,.T.);
#4722=EDGE_CURVE('',#4013,#4014,#2533,.T.);
#4723=EDGE_CURVE('',#4014,#4014,#3508,.T.);
#4724=EDGE_CURVE('',#4015,#4015,#3509,.T.);
#4725=EDGE_CURVE('',#4015,#4016,#2534,.T.);
#4726=EDGE_CURVE('',#4016,#4016,#3510,.T.);
#4727=EDGE_CURVE('',#4017,#4017,#3511,.T.);
#4728=EDGE_CURVE('',#4017,#4018,#2535,.T.);
#4729=EDGE_CURVE('',#4018,#4018,#3512,.T.);
#4730=EDGE_CURVE('',#4019,#4019,#3513,.T.);
#4731=EDGE_CURVE('',#4019,#4020,#2536,.T.);
#4732=EDGE_CURVE('',#4020,#4020,#3514,.T.);
#4733=EDGE_CURVE('',#4012,#4010,#3515,.T.);
#4734=EDGE_CURVE('',#4011,#4012,#2537,.T.);
#4735=EDGE_CURVE('',#4009,#4011,#3516,.T.);
#4736=EDGE_CURVE('',#4021,#4021,#3517,.T.);
#4737=EDGE_CURVE('',#4008,#4006,#3518,.T.);
#4738=EDGE_CURVE('',#4007,#4008,#2538,.T.);
#4739=EDGE_CURVE('',#4005,#4007,#3519,.T.);
#4740=EDGE_CURVE('',#4022,#4022,#3520,.T.);
#4741=EDGE_CURVE('',#4004,#4002,#3521,.T.);
#4742=EDGE_CURVE('',#4003,#4004,#2539,.T.);
#4743=EDGE_CURVE('',#4001,#4003,#3522,.T.);
#4744=EDGE_CURVE('',#4023,#4023,#3523,.T.);
#4745=EDGE_CURVE('',#4000,#3998,#3524,.T.);
#4746=EDGE_CURVE('',#3999,#4000,#2540,.T.);
#4747=EDGE_CURVE('',#3997,#3999,#3525,.T.);
#4748=EDGE_CURVE('',#4024,#4024,#3526,.T.);
#4749=EDGE_CURVE('',#4008,#4012,#3527,.T.);
#4750=EDGE_CURVE('',#4012,#4000,#3528,.T.);
#4751=EDGE_CURVE('',#4000,#4004,#3529,.T.);
#4752=EDGE_CURVE('',#4004,#4008,#3530,.T.);
#4753=EDGE_CURVE('',#4025,#4025,#3531,.T.);
#4754=EDGE_CURVE('',#4026,#4026,#3532,.T.);
#4755=EDGE_CURVE('',#4026,#4021,#2541,.T.);
#4756=EDGE_CURVE('',#4027,#4027,#3533,.T.);
#4757=EDGE_CURVE('',#4027,#4022,#2542,.T.);
#4758=EDGE_CURVE('',#4028,#4028,#3534,.T.);
#4759=EDGE_CURVE('',#4028,#4023,#2543,.T.);
#4760=EDGE_CURVE('',#4029,#4029,#3535,.T.);
#4761=EDGE_CURVE('',#4029,#4024,#2544,.T.);
#4762=EDGE_CURVE('',#4025,#4030,#2545,.T.);
#4763=EDGE_CURVE('',#4030,#4030,#3536,.T.);
#4764=EDGE_CURVE('',#4031,#4031,#3537,.T.);
#4765=EDGE_CURVE('',#4031,#4032,#2546,.T.);
#4766=EDGE_CURVE('',#4032,#4032,#3538,.T.);
#4767=EDGE_CURVE('',#4007,#4033,#2547,.T.);
#4768=EDGE_CURVE('',#4033,#4033,#3539,.T.);
#4769=EDGE_CURVE('',#4034,#4034,#3540,.T.);
#4770=EDGE_CURVE('',#4034,#4035,#2548,.T.);
#4771=EDGE_CURVE('',#4035,#4035,#3541,.T.);
#4772=EDGE_CURVE('',#4036,#4036,#3542,.T.);
#4773=EDGE_CURVE('',#4036,#4037,#2549,.T.);
#4774=EDGE_CURVE('',#4037,#4037,#3543,.T.);
#4775=EDGE_CURVE('',#4038,#4038,#3544,.T.);
#4776=EDGE_CURVE('',#4038,#4039,#2550,.T.);
#4777=EDGE_CURVE('',#4039,#4039,#3545,.T.);
#4778=EDGE_CURVE('',#4040,#4040,#3546,.T.);
#4779=EDGE_CURVE('',#4040,#4041,#2551,.T.);
#4780=EDGE_CURVE('',#4041,#4041,#3547,.T.);
#4781=EDGE_CURVE('',#4042,#4042,#3548,.T.);
#4782=EDGE_CURVE('',#4042,#4043,#2552,.T.);
#4783=EDGE_CURVE('',#4043,#4043,#3549,.T.);
#4784=EDGE_CURVE('',#4044,#4044,#3550,.T.);
#4785=EDGE_CURVE('',#4045,#4045,#3551,.T.);
#4786=EDGE_CURVE('',#4045,#4044,#2553,.T.);
#4787=EDGE_CURVE('',#4046,#4046,#3552,.T.);
#4788=EDGE_CURVE('',#4046,#4047,#2554,.T.);
#4789=EDGE_CURVE('',#4047,#4047,#3553,.T.);
#4790=EDGE_CURVE('',#4048,#4049,#2555,.T.);
#4791=EDGE_CURVE('',#4049,#4050,#2556,.T.);
#4792=EDGE_CURVE('',#4050,#4051,#2557,.T.);
#4793=EDGE_CURVE('',#4048,#4051,#2558,.T.);
#4794=EDGE_CURVE('',#4049,#4052,#2559,.T.);
#4795=EDGE_CURVE('',#4052,#4053,#2560,.T.);
#4796=EDGE_CURVE('',#4053,#4050,#2561,.T.);
#4797=EDGE_CURVE('',#4052,#4054,#2562,.T.);
#4798=EDGE_CURVE('',#4054,#4055,#2563,.T.);
#4799=EDGE_CURVE('',#4055,#4053,#2564,.T.);
#4800=EDGE_CURVE('',#4054,#4056,#2565,.T.);
#4801=EDGE_CURVE('',#4056,#4057,#2566,.T.);
#4802=EDGE_CURVE('',#4057,#4055,#2567,.T.);
#4803=EDGE_CURVE('',#4056,#4058,#2568,.T.);
#4804=EDGE_CURVE('',#4058,#4059,#2569,.T.);
#4805=EDGE_CURVE('',#4059,#4057,#2570,.T.);
#4806=EDGE_CURVE('',#4058,#4048,#2571,.T.);
#4807=EDGE_CURVE('',#4051,#4059,#2572,.T.);
#4808=EDGE_CURVE('',#4060,#4060,#3554,.T.);
#4809=EDGE_CURVE('',#4061,#4061,#3555,.T.);
#4810=EDGE_CURVE('',#4062,#4062,#3556,.T.);
#4811=EDGE_CURVE('',#4062,#4061,#2573,.T.);
#4812=EDGE_CURVE('',#4063,#4063,#3557,.T.);
#4813=EDGE_CURVE('',#4063,#4062,#2574,.T.);
#4814=EDGE_CURVE('',#4064,#4064,#3558,.T.);
#4815=EDGE_CURVE('',#4064,#4063,#2575,.T.);
#4816=EDGE_CURVE('',#4065,#4065,#3559,.T.);
#4817=EDGE_CURVE('',#4066,#4066,#3560,.F.);
#4818=EDGE_CURVE('',#4066,#4065,#2576,.T.);
#4819=EDGE_CURVE('',#4060,#4066,#2577,.T.);
#4820=EDGE_CURVE('',#4067,#4068,#3561,.T.);
#4821=EDGE_CURVE('',#4068,#4067,#3562,.T.);
#4822=EDGE_CURVE('',#4068,#4069,#3563,.T.);
#4823=EDGE_CURVE('',#4070,#4069,#3564,.T.);
#4824=EDGE_CURVE('',#4069,#4070,#3565,.T.);
#4825=EDGE_CURVE('',#4070,#4071,#2578,.T.);
#4826=EDGE_CURVE('',#4071,#4071,#3566,.T.);
#4827=EDGE_CURVE('',#4072,#4072,#3567,.T.);
#4828=EDGE_CURVE('',#4072,#4073,#2579,.T.);
#4829=EDGE_CURVE('',#4073,#4073,#3568,.T.);
#4830=EDGE_CURVE('',#4073,#4074,#2580,.T.);
#4831=EDGE_CURVE('',#4074,#4074,#3569,.T.);
#4832=EDGE_CURVE('',#4075,#4075,#3570,.T.);
#4833=EDGE_CURVE('',#4075,#4067,#2581,.T.);
#4834=EDGE_CURVE('',#4076,#4076,#3571,.T.);
#4835=EDGE_CURVE('',#4076,#4072,#2582,.T.);
#4836=EDGE_CURVE('',#4077,#4078,#3572,.T.);
#4837=EDGE_CURVE('',#4078,#4077,#3573,.T.);
#4838=EDGE_CURVE('',#4078,#4079,#3574,.T.);
#4839=EDGE_CURVE('',#4080,#4079,#3575,.T.);
#4840=EDGE_CURVE('',#4079,#4080,#3576,.T.);
#4841=EDGE_CURVE('',#4081,#4081,#3577,.T.);
#4842=EDGE_CURVE('',#4081,#4080,#2583,.T.);
#4843=EDGE_CURVE('',#4082,#4082,#3578,.T.);
#4844=EDGE_CURVE('',#4083,#4083,#3579,.T.);
#4845=EDGE_CURVE('',#4084,#4084,#3580,.T.);
#4846=EDGE_CURVE('',#4084,#4082,#2584,.T.);
#4847=EDGE_CURVE('',#4085,#4085,#3581,.T.);
#4848=EDGE_CURVE('',#4085,#4084,#2585,.T.);
#4849=EDGE_CURVE('',#4086,#4086,#3582,.T.);
#4850=EDGE_CURVE('',#4086,#4085,#2586,.T.);
#4851=EDGE_CURVE('',#4077,#4083,#2587,.T.);
#4852=EDGE_CURVE('',#4087,#4088,#3583,.T.);
#4853=EDGE_CURVE('',#4089,#4090,#3584,.T.);
#4854=EDGE_CURVE('',#4091,#4092,#3585,.T.);
#4855=EDGE_CURVE('',#4093,#4094,#3586,.T.);
#4856=EDGE_CURVE('',#4095,#4096,#3587,.T.);
#4857=EDGE_CURVE('',#4097,#4098,#3588,.T.);
#4858=EDGE_CURVE('',#4099,#4100,#3589,.T.);
#4859=EDGE_CURVE('',#4101,#4102,#3590,.T.);
#4860=EDGE_CURVE('',#4103,#4104,#3591,.T.);
#4861=EDGE_CURVE('',#4105,#4106,#399,.T.);
#4862=EDGE_CURVE('',#4107,#4105,#3592,.T.);
#4863=EDGE_CURVE('',#4108,#4107,#400,.T.);
#4864=EDGE_CURVE('',#4106,#4108,#3593,.T.);
#4865=EDGE_CURVE('',#4109,#4107,#3594,.T.);
#4866=EDGE_CURVE('',#4109,#4110,#401,.T.);
#4867=EDGE_CURVE('',#4111,#4110,#3595,.T.);
#4868=EDGE_CURVE('',#4111,#4112,#402,.T.);
#4869=EDGE_CURVE('',#4113,#4112,#3596,.T.);
#4870=EDGE_CURVE('',#4113,#4114,#403,.T.);
#4871=EDGE_CURVE('',#4115,#4114,#3597,.T.);
#4872=EDGE_CURVE('',#4115,#4116,#2588,.T.);
#4873=EDGE_CURVE('',#4116,#4116,#3598,.T.);
#4874=EDGE_CURVE('',#4117,#4115,#3599,.T.);
#4875=EDGE_CURVE('',#4117,#4118,#404,.T.);
#4876=EDGE_CURVE('',#4119,#4118,#3600,.T.);
#4877=EDGE_CURVE('',#4119,#4120,#405,.T.);
#4878=EDGE_CURVE('',#4121,#4120,#3601,.T.);
#4879=EDGE_CURVE('',#4121,#4122,#406,.T.);
#4880=EDGE_CURVE('',#4123,#4122,#3602,.T.);
#4881=EDGE_CURVE('',#4123,#4124,#407,.T.);
#4882=EDGE_CURVE('',#4125,#4124,#3603,.T.);
#4883=EDGE_CURVE('',#4125,#4126,#408,.T.);
#4884=EDGE_CURVE('',#4108,#4126,#3604,.T.);
#4885=EDGE_CURVE('',#4105,#4127,#3605,.T.);
#4886=EDGE_CURVE('',#4127,#4109,#3606,.T.);
#4887=EDGE_CURVE('',#4128,#4127,#409,.T.);
#4888=EDGE_CURVE('',#4110,#4128,#3607,.T.);
#4889=EDGE_CURVE('',#4128,#4129,#3608,.T.);
#4890=EDGE_CURVE('',#4129,#4111,#3609,.T.);
#4891=EDGE_CURVE('',#4130,#4129,#410,.T.);
#4892=EDGE_CURVE('',#4112,#4130,#3610,.T.);
#4893=EDGE_CURVE('',#4130,#4131,#3611,.T.);
#4894=EDGE_CURVE('',#4131,#4113,#3612,.T.);
#4895=EDGE_CURVE('',#4132,#4131,#411,.T.);
#4896=EDGE_CURVE('',#4114,#4132,#3613,.T.);
#4897=EDGE_CURVE('',#4132,#4133,#3614,.T.);
#4898=EDGE_CURVE('',#4133,#4134,#3615,.T.);
#4899=EDGE_CURVE('',#4134,#4117,#3616,.T.);
#4900=EDGE_CURVE('',#4135,#4134,#412,.T.);
#4901=EDGE_CURVE('',#4118,#4135,#3617,.T.);
#4902=EDGE_CURVE('',#4135,#4136,#3618,.T.);
#4903=EDGE_CURVE('',#4136,#4119,#3619,.T.);
#4904=EDGE_CURVE('',#4137,#4136,#413,.T.);
#4905=EDGE_CURVE('',#4120,#4137,#3620,.T.);
#4906=EDGE_CURVE('',#4137,#4138,#3621,.T.);
#4907=EDGE_CURVE('',#4138,#4121,#3622,.T.);
#4908=EDGE_CURVE('',#4139,#4138,#414,.T.);
#4909=EDGE_CURVE('',#4122,#4139,#3623,.T.);
#4910=EDGE_CURVE('',#4139,#4140,#3624,.T.);
#4911=EDGE_CURVE('',#4140,#4123,#3625,.T.);
#4912=EDGE_CURVE('',#4141,#4140,#415,.T.);
#4913=EDGE_CURVE('',#4124,#4141,#3626,.T.);
#4914=EDGE_CURVE('',#4142,#4142,#3627,.T.);
#4915=EDGE_CURVE('',#4142,#4133,#2589,.T.);
#4916=EDGE_CURVE('',#4143,#4106,#3628,.T.);
#4917=EDGE_CURVE('',#4143,#4144,#416,.T.);
#4918=EDGE_CURVE('',#4141,#4144,#3629,.T.);
#4919=EDGE_CURVE('',#4126,#4143,#3630,.T.);
#4920=EDGE_CURVE('',#4144,#4125,#3631,.T.);
#4921=EDGE_CURVE('',#4145,#4145,#3632,.T.);
#4922=EDGE_CURVE('',#4146,#4146,#3633,.T.);
#4923=EDGE_CURVE('',#4147,#4147,#3634,.T.);
#4924=EDGE_CURVE('',#4147,#4145,#2590,.T.);
#4925=EDGE_CURVE('',#4148,#4148,#3635,.T.);
#4926=EDGE_CURVE('',#4148,#4146,#2591,.T.);
#4927=EDGE_CURVE('',#4149,#4149,#3636,.T.);
#4928=EDGE_CURVE('',#4150,#4150,#3637,.T.);
#4929=EDGE_CURVE('',#4151,#4151,#3638,.T.);
#4930=EDGE_CURVE('',#4151,#4149,#2592,.T.);
#4931=EDGE_CURVE('',#4152,#4152,#3639,.T.);
#4932=EDGE_CURVE('',#4152,#4150,#2593,.T.);
#4933=EDGE_CURVE('',#4153,#4154,#2594,.T.);
#4934=EDGE_CURVE('',#4154,#4155,#2595,.T.);
#4935=EDGE_CURVE('',#4156,#4155,#2596,.T.);
#4936=EDGE_CURVE('',#4153,#4156,#2597,.T.);
#4937=EDGE_CURVE('',#4157,#4153,#2598,.T.);
#4938=EDGE_CURVE('',#4158,#4156,#2599,.T.);
#4939=EDGE_CURVE('',#4157,#4158,#2600,.T.);
#4940=EDGE_CURVE('',#4159,#4157,#2601,.T.);
#4941=EDGE_CURVE('',#4160,#4158,#2602,.T.);
#4942=EDGE_CURVE('',#4159,#4160,#2603,.T.);
#4943=EDGE_CURVE('',#4154,#4159,#2604,.T.);
#4944=EDGE_CURVE('',#4155,#4160,#2605,.T.);
#4945=EDGE_CURVE('',#4161,#4162,#2606,.T.);
#4946=EDGE_CURVE('',#4162,#4163,#2607,.T.);
#4947=EDGE_CURVE('',#4164,#4163,#2608,.T.);
#4948=EDGE_CURVE('',#4161,#4164,#2609,.T.);
#4949=EDGE_CURVE('',#4165,#4161,#2610,.T.);
#4950=EDGE_CURVE('',#4166,#4164,#2611,.T.);
#4951=EDGE_CURVE('',#4165,#4166,#2612,.T.);
#4952=EDGE_CURVE('',#4167,#4165,#2613,.T.);
#4953=EDGE_CURVE('',#4168,#4166,#2614,.T.);
#4954=EDGE_CURVE('',#4167,#4168,#2615,.T.);
#4955=EDGE_CURVE('',#4162,#4167,#2616,.T.);
#4956=EDGE_CURVE('',#4163,#4168,#2617,.T.);
#4957=EDGE_CURVE('',#4169,#4169,#3640,.T.);
#4958=EDGE_CURVE('',#4169,#4170,#2618,.T.);
#4959=EDGE_CURVE('',#4170,#4170,#3641,.T.);
#4960=EDGE_CURVE('',#4171,#4171,#3642,.T.);
#4961=EDGE_CURVE('',#4171,#4172,#2619,.T.);
#4962=EDGE_CURVE('',#4172,#4172,#3643,.T.);
#4963=EDGE_CURVE('',#4173,#4173,#3644,.T.);
#4964=EDGE_CURVE('',#4173,#4174,#2620,.T.);
#4965=EDGE_CURVE('',#4174,#4174,#3645,.T.);
#4966=EDGE_CURVE('',#4175,#4175,#3646,.T.);
#4967=EDGE_CURVE('',#4176,#4176,#3647,.T.);
#4968=EDGE_CURVE('',#4177,#4177,#3648,.T.);
#4969=EDGE_CURVE('',#4177,#4175,#2621,.T.);
#4970=EDGE_CURVE('',#4176,#4178,#2622,.T.);
#4971=EDGE_CURVE('',#4178,#4178,#3649,.T.);
#4972=EDGE_CURVE('',#4179,#4179,#3650,.T.);
#4973=EDGE_CURVE('',#4179,#4180,#2623,.T.);
#4974=EDGE_CURVE('',#4180,#4180,#3651,.T.);
#4975=EDGE_CURVE('',#4181,#4181,#3652,.T.);
#4976=EDGE_CURVE('',#4181,#4182,#2624,.T.);
#4977=EDGE_CURVE('',#4182,#4182,#3653,.T.);
#4978=EDGE_CURVE('',#4183,#4183,#3654,.T.);
#4979=EDGE_CURVE('',#4183,#4184,#2625,.T.);
#4980=EDGE_CURVE('',#4184,#4184,#3655,.T.);
#4981=EDGE_CURVE('',#4185,#4185,#3656,.T.);
#4982=EDGE_CURVE('',#4185,#4186,#2626,.T.);
#4983=EDGE_CURVE('',#4186,#4186,#3657,.T.);
#4984=EDGE_CURVE('',#4187,#4187,#3658,.T.);
#4985=EDGE_CURVE('',#4187,#4188,#2627,.T.);
#4986=EDGE_CURVE('',#4188,#4188,#3659,.T.);
#4987=EDGE_CURVE('',#4189,#4189,#3660,.T.);
#4988=EDGE_CURVE('',#4189,#4190,#2628,.T.);
#4989=EDGE_CURVE('',#4190,#4190,#3661,.T.);
#4990=EDGE_CURVE('',#4191,#4191,#3662,.T.);
#4991=EDGE_CURVE('',#4191,#4192,#2629,.T.);
#4992=EDGE_CURVE('',#4192,#4192,#3663,.T.);
#4993=EDGE_CURVE('',#4193,#4193,#3664,.T.);
#4994=EDGE_CURVE('',#4193,#4194,#2630,.T.);
#4995=EDGE_CURVE('',#4194,#4194,#3665,.T.);
#4996=EDGE_CURVE('',#4195,#4195,#3666,.T.);
#4997=EDGE_CURVE('',#4195,#4196,#2631,.T.);
#4998=EDGE_CURVE('',#4196,#4196,#3667,.T.);
#4999=EDGE_CURVE('',#4197,#4197,#3668,.T.);
#5000=EDGE_CURVE('',#4197,#4198,#2632,.T.);
#5001=EDGE_CURVE('',#4198,#4198,#3669,.T.);
#5002=EDGE_CURVE('',#4199,#4199,#3670,.T.);
#5003=EDGE_CURVE('',#4199,#4200,#2633,.T.);
#5004=EDGE_CURVE('',#4200,#4200,#3671,.T.);
#5005=EDGE_CURVE('',#4201,#4201,#3672,.T.);
#5006=EDGE_CURVE('',#4201,#4202,#2634,.T.);
#5007=EDGE_CURVE('',#4202,#4202,#3673,.T.);
#5008=EDGE_CURVE('',#4203,#4203,#3674,.T.);
#5009=EDGE_CURVE('',#4203,#4204,#2635,.T.);
#5010=EDGE_CURVE('',#4204,#4204,#3675,.T.);
#5011=EDGE_CURVE('',#4205,#4206,#2636,.T.);
#5012=EDGE_CURVE('',#4205,#4207,#3676,.T.);
#5013=EDGE_CURVE('',#4207,#4206,#3677,.T.);
#5014=EDGE_CURVE('',#4208,#4205,#417,.T.);
#5015=EDGE_CURVE('',#4209,#4208,#3678,.T.);
#5016=EDGE_CURVE('',#4206,#4209,#418,.T.);
#5017=EDGE_CURVE('',#4207,#4210,#2637,.T.);
#5018=EDGE_CURVE('',#4210,#4210,#419,.T.);
#5019=EDGE_CURVE('',#4209,#4208,#2638,.T.);
#5020=EDGE_CURVE('',#4211,#4211,#3679,.T.);
#5021=EDGE_CURVE('',#4211,#4212,#2639,.T.);
#5022=EDGE_CURVE('',#4212,#4212,#3680,.T.);
#5023=EDGE_CURVE('',#4213,#4213,#3681,.T.);
#5024=EDGE_CURVE('',#4213,#4214,#2640,.T.);
#5025=EDGE_CURVE('',#4214,#4214,#3682,.T.);
#5026=EDGE_CURVE('',#4215,#4215,#3683,.T.);
#5027=EDGE_CURVE('',#4216,#4216,#3684,.T.);
#5028=EDGE_CURVE('',#4216,#4215,#2641,.T.);
#5029=EDGE_CURVE('',#4217,#4217,#3685,.T.);
#5030=EDGE_CURVE('',#4217,#4216,#2642,.T.);
#5031=EDGE_CURVE('',#4218,#4218,#3686,.T.);
#5032=EDGE_CURVE('',#4218,#4217,#2643,.T.);
#5033=EDGE_CURVE('',#4219,#4219,#3687,.T.);
#5034=EDGE_CURVE('',#4220,#4220,#3688,.F.);
#5035=EDGE_CURVE('',#4220,#4219,#2644,.T.);
#5036=EDGE_CURVE('',#4221,#4221,#3689,.F.);
#5037=EDGE_CURVE('',#4221,#4220,#2645,.T.);
#5038=EDGE_CURVE('',#4222,#4222,#3690,.T.);
#5039=EDGE_CURVE('',#4222,#4221,#2646,.T.);
#5040=EDGE_CURVE('',#4223,#4224,#2647,.T.);
#5041=EDGE_CURVE('',#4224,#4225,#2648,.T.);
#5042=EDGE_CURVE('',#4225,#4226,#2649,.T.);
#5043=EDGE_CURVE('',#4223,#4226,#2650,.T.);
#5044=EDGE_CURVE('',#4224,#4227,#2651,.T.);
#5045=EDGE_CURVE('',#4227,#4228,#2652,.T.);
#5046=EDGE_CURVE('',#4228,#4225,#2653,.T.);
#5047=EDGE_CURVE('',#4227,#4229,#2654,.T.);
#5048=EDGE_CURVE('',#4229,#4230,#2655,.T.);
#5049=EDGE_CURVE('',#4230,#4228,#2656,.T.);
#5050=EDGE_CURVE('',#4229,#4231,#2657,.T.);
#5051=EDGE_CURVE('',#4231,#4232,#2658,.T.);
#5052=EDGE_CURVE('',#4232,#4230,#2659,.T.);
#5053=EDGE_CURVE('',#4231,#4233,#2660,.T.);
#5054=EDGE_CURVE('',#4233,#4234,#2661,.T.);
#5055=EDGE_CURVE('',#4234,#4232,#2662,.T.);
#5056=EDGE_CURVE('',#4233,#4223,#2663,.T.);
#5057=EDGE_CURVE('',#4226,#4234,#2664,.T.);
#5058=EDGE_CURVE('',#4235,#4236,#2665,.T.);
#5059=EDGE_CURVE('',#4235,#4237,#2666,.T.);
#5060=EDGE_CURVE('',#4237,#4238,#2667,.T.);
#5061=EDGE_CURVE('',#4236,#4238,#2668,.T.);
#5062=EDGE_CURVE('',#4239,#4235,#2669,.T.);
#5063=EDGE_CURVE('',#4239,#4240,#2670,.T.);
#5064=EDGE_CURVE('',#4240,#4237,#2671,.T.);
#5065=EDGE_CURVE('',#4241,#4239,#2672,.T.);
#5066=EDGE_CURVE('',#4241,#4242,#2673,.T.);
#5067=EDGE_CURVE('',#4242,#4240,#2674,.T.);
#5068=EDGE_CURVE('',#4243,#4241,#2675,.T.);
#5069=EDGE_CURVE('',#4243,#4244,#2676,.T.);
#5070=EDGE_CURVE('',#4244,#4242,#2677,.T.);
#5071=EDGE_CURVE('',#4245,#4243,#2678,.T.);
#5072=EDGE_CURVE('',#4245,#4246,#2679,.T.);
#5073=EDGE_CURVE('',#4246,#4244,#2680,.T.);
#5074=EDGE_CURVE('',#4236,#4245,#2681,.T.);
#5075=EDGE_CURVE('',#4238,#4246,#2682,.T.);
#5076=EDGE_CURVE('',#4247,#4247,#3691,.T.);
#5077=EDGE_CURVE('',#4248,#4248,#3692,.T.);
#5078=EDGE_CURVE('',#4248,#4247,#2683,.T.);
#5079=EDGE_CURVE('',#4249,#4249,#3693,.F.);
#5080=EDGE_CURVE('',#4249,#4248,#2684,.T.);
#5081=EDGE_CURVE('',#4250,#4250,#3694,.T.);
#5082=EDGE_CURVE('',#4250,#4249,#2685,.T.);
#5083=EDGE_CURVE('',#4251,#4251,#3695,.T.);
#5084=EDGE_CURVE('',#4251,#4252,#2686,.T.);
#5085=EDGE_CURVE('',#4252,#4252,#3696,.T.);
#5086=EDGE_CURVE('',#4253,#4253,#3697,.T.);
#5087=EDGE_CURVE('',#4253,#4254,#2687,.T.);
#5088=EDGE_CURVE('',#4254,#4254,#3698,.T.);
#5089=EDGE_CURVE('',#4255,#4255,#3699,.T.);
#5090=EDGE_CURVE('',#4255,#4256,#2688,.T.);
#5091=EDGE_CURVE('',#4256,#4256,#3700,.T.);
#5092=EDGE_CURVE('',#4257,#4257,#3701,.T.);
#5093=EDGE_CURVE('',#4257,#4258,#2689,.T.);
#5094=EDGE_CURVE('',#4258,#4258,#3702,.T.);
#5095=EDGE_CURVE('',#4259,#4259,#3703,.T.);
#5096=EDGE_CURVE('',#4259,#4260,#2690,.T.);
#5097=EDGE_CURVE('',#4260,#4260,#3704,.T.);
#5098=EDGE_CURVE('',#4261,#4261,#3705,.T.);
#5099=EDGE_CURVE('',#4261,#4262,#2691,.T.);
#5100=EDGE_CURVE('',#4262,#4262,#3706,.T.);
#5101=EDGE_CURVE('',#4263,#4264,#2692,.T.);
#5102=EDGE_CURVE('',#4263,#4265,#2693,.T.);
#5103=EDGE_CURVE('',#4266,#4265,#2694,.T.);
#5104=EDGE_CURVE('',#4264,#4266,#2695,.T.);
#5105=EDGE_CURVE('',#4267,#4268,#2696,.T.);
#5106=EDGE_CURVE('',#4269,#4267,#2697,.T.);
#5107=EDGE_CURVE('',#4270,#4269,#2698,.T.);
#5108=EDGE_CURVE('',#4268,#4270,#2699,.T.);
#5109=EDGE_CURVE('',#4268,#4263,#2700,.T.);
#5110=EDGE_CURVE('',#4265,#4270,#2701,.T.);
#5111=EDGE_CURVE('',#4266,#4269,#2702,.T.);
#5112=EDGE_CURVE('',#4267,#4264,#2703,.T.);
#5113=EDGE_CURVE('',#4271,#4272,#2704,.T.);
#5114=EDGE_CURVE('',#4271,#4273,#2705,.T.);
#5115=EDGE_CURVE('',#4274,#4273,#2706,.T.);
#5116=EDGE_CURVE('',#4272,#4274,#2707,.T.);
#5117=EDGE_CURVE('',#4275,#4276,#2708,.T.);
#5118=EDGE_CURVE('',#4277,#4275,#2709,.T.);
#5119=EDGE_CURVE('',#4278,#4277,#2710,.T.);
#5120=EDGE_CURVE('',#4276,#4278,#2711,.T.);
#5121=EDGE_CURVE('',#4276,#4271,#2712,.T.);
#5122=EDGE_CURVE('',#4273,#4278,#2713,.T.);
#5123=EDGE_CURVE('',#4274,#4277,#2714,.T.);
#5124=EDGE_CURVE('',#4275,#4272,#2715,.T.);
#5125=EDGE_CURVE('',#4279,#4280,#2716,.T.);
#5126=EDGE_CURVE('',#4280,#4281,#2717,.T.);
#5127=EDGE_CURVE('',#4282,#4281,#2718,.T.);
#5128=EDGE_CURVE('',#4279,#4282,#2719,.T.);
#5129=EDGE_CURVE('',#4283,#4279,#2720,.T.);
#5130=EDGE_CURVE('',#4284,#4282,#2721,.T.);
#5131=EDGE_CURVE('',#4283,#4284,#2722,.T.);
#5132=EDGE_CURVE('',#4285,#4283,#2723,.T.);
#5133=EDGE_CURVE('',#4286,#4284,#2724,.T.);
#5134=EDGE_CURVE('',#4285,#4286,#2725,.T.);
#5135=EDGE_CURVE('',#4280,#4285,#2726,.T.);
#5136=EDGE_CURVE('',#4281,#4286,#2727,.T.);
#5137=EDGE_CURVE('',#4287,#4287,#3707,.T.);
#5138=EDGE_CURVE('',#4287,#4288,#2728,.T.);
#5139=EDGE_CURVE('',#4288,#4288,#3708,.T.);
#5140=EDGE_CURVE('',#4289,#4289,#3709,.T.);
#5141=EDGE_CURVE('',#4290,#4290,#3710,.T.);
#5142=EDGE_CURVE('',#4289,#4291,#2729,.T.);
#5143=EDGE_CURVE('',#4291,#4291,#3711,.T.);
#5144=EDGE_CURVE('',#4292,#4292,#3712,.T.);
#5145=EDGE_CURVE('',#4292,#4290,#2730,.T.);
#5146=EDGE_CURVE('',#4293,#4293,#3713,.T.);
#5147=EDGE_CURVE('',#4293,#4294,#2731,.T.);
#5148=EDGE_CURVE('',#4294,#4294,#3714,.T.);
#5149=EDGE_CURVE('',#4295,#4295,#3715,.T.);
#5150=EDGE_CURVE('',#4295,#4296,#2732,.T.);
#5151=EDGE_CURVE('',#4296,#4296,#3716,.T.);
#5152=EDGE_CURVE('',#4297,#4297,#3717,.T.);
#5153=EDGE_CURVE('',#4297,#4298,#2733,.T.);
#5154=EDGE_CURVE('',#4298,#4298,#3718,.T.);
#5155=EDGE_CURVE('',#4299,#4299,#3719,.T.);
#5156=EDGE_CURVE('',#4299,#4300,#2734,.T.);
#5157=EDGE_CURVE('',#4300,#4300,#3720,.T.);
#5158=EDGE_CURVE('',#4301,#4301,#3721,.T.);
#5159=EDGE_CURVE('',#4301,#4302,#2735,.T.);
#5160=EDGE_CURVE('',#4302,#4302,#3722,.T.);
#5161=EDGE_CURVE('',#4303,#4303,#3723,.T.);
#5162=EDGE_CURVE('',#4303,#4304,#2736,.T.);
#5163=EDGE_CURVE('',#4304,#4304,#3724,.T.);
#5164=EDGE_CURVE('',#4305,#4305,#3725,.T.);
#5165=EDGE_CURVE('',#4305,#4306,#2737,.T.);
#5166=EDGE_CURVE('',#4306,#4306,#3726,.T.);
#5167=EDGE_CURVE('',#4307,#4307,#3727,.T.);
#5168=EDGE_CURVE('',#4307,#4308,#2738,.T.);
#5169=EDGE_CURVE('',#4308,#4308,#3728,.T.);
#5170=EDGE_CURVE('',#4309,#4309,#3729,.T.);
#5171=EDGE_CURVE('',#4309,#4310,#2739,.T.);
#5172=EDGE_CURVE('',#4310,#4310,#3730,.T.);
#5173=EDGE_CURVE('',#4311,#4311,#3731,.T.);
#5174=EDGE_CURVE('',#4311,#4312,#2740,.T.);
#5175=EDGE_CURVE('',#4312,#4312,#3732,.T.);
#5176=EDGE_CURVE('',#4313,#4313,#3733,.T.);
#5177=EDGE_CURVE('',#4313,#4314,#2741,.T.);
#5178=EDGE_CURVE('',#4314,#4314,#3734,.T.);
#5179=EDGE_CURVE('',#4315,#4315,#3735,.T.);
#5180=EDGE_CURVE('',#4315,#4316,#2742,.T.);
#5181=EDGE_CURVE('',#4316,#4316,#3736,.T.);
#5182=EDGE_CURVE('',#4317,#4318,#2743,.T.);
#5183=EDGE_CURVE('',#4317,#4319,#2744,.T.);
#5184=EDGE_CURVE('',#4320,#4319,#2745,.T.);
#5185=EDGE_CURVE('',#4318,#4320,#2746,.T.);
#5186=EDGE_CURVE('',#4321,#4322,#2747,.T.);
#5187=EDGE_CURVE('',#4323,#4321,#2748,.T.);
#5188=EDGE_CURVE('',#4324,#4323,#2749,.T.);
#5189=EDGE_CURVE('',#4322,#4324,#2750,.T.);
#5190=EDGE_CURVE('',#4322,#4317,#2751,.T.);
#5191=EDGE_CURVE('',#4319,#4324,#2752,.T.);
#5192=EDGE_CURVE('',#4320,#4323,#2753,.T.);
#5193=EDGE_CURVE('',#4321,#4318,#2754,.T.);
#5194=EDGE_CURVE('',#4325,#4326,#2755,.T.);
#5195=EDGE_CURVE('',#4325,#4327,#2756,.T.);
#5196=EDGE_CURVE('',#4328,#4327,#2757,.T.);
#5197=EDGE_CURVE('',#4326,#4328,#2758,.T.);
#5198=EDGE_CURVE('',#4329,#4330,#2759,.T.);
#5199=EDGE_CURVE('',#4331,#4329,#2760,.T.);
#5200=EDGE_CURVE('',#4332,#4331,#2761,.T.);
#5201=EDGE_CURVE('',#4330,#4332,#2762,.T.);
#5202=EDGE_CURVE('',#4330,#4325,#2763,.T.);
#5203=EDGE_CURVE('',#4327,#4332,#2764,.T.);
#5204=EDGE_CURVE('',#4328,#4331,#2765,.T.);
#5205=EDGE_CURVE('',#4329,#4326,#2766,.T.);
#5206=EDGE_CURVE('',#4333,#4334,#2767,.T.);
#5207=EDGE_CURVE('',#4334,#4335,#2768,.T.);
#5208=EDGE_CURVE('',#4336,#4335,#2769,.T.);
#5209=EDGE_CURVE('',#4333,#4336,#2770,.T.);
#5210=EDGE_CURVE('',#4337,#4333,#2771,.T.);
#5211=EDGE_CURVE('',#4338,#4336,#2772,.T.);
#5212=EDGE_CURVE('',#4337,#4338,#2773,.T.);
#5213=EDGE_CURVE('',#4339,#4337,#2774,.T.);
#5214=EDGE_CURVE('',#4340,#4338,#2775,.T.);
#5215=EDGE_CURVE('',#4339,#4340,#2776,.T.);
#5216=EDGE_CURVE('',#4334,#4339,#2777,.T.);
#5217=EDGE_CURVE('',#4335,#4340,#2778,.T.);
#5218=EDGE_CURVE('',#4341,#4341,#3737,.T.);
#5219=EDGE_CURVE('',#4341,#4342,#2779,.T.);
#5220=EDGE_CURVE('',#4342,#4342,#3738,.T.);
#5221=EDGE_CURVE('',#4343,#4343,#3739,.T.);
#5222=EDGE_CURVE('',#4344,#4344,#3740,.T.);
#5223=EDGE_CURVE('',#4343,#4345,#2780,.T.);
#5224=EDGE_CURVE('',#4345,#4345,#3741,.T.);
#5225=EDGE_CURVE('',#4346,#4346,#3742,.T.);
#5226=EDGE_CURVE('',#4346,#4344,#2781,.T.);
#5227=EDGE_CURVE('',#4347,#4347,#3743,.T.);
#5228=EDGE_CURVE('',#4347,#4348,#2782,.T.);
#5229=EDGE_CURVE('',#4348,#4348,#3744,.T.);
#5230=EDGE_CURVE('',#4349,#4349,#3745,.T.);
#5231=EDGE_CURVE('',#4349,#4350,#2783,.T.);
#5232=EDGE_CURVE('',#4350,#4350,#3746,.T.);
#5233=EDGE_CURVE('',#4351,#4351,#3747,.T.);
#5234=EDGE_CURVE('',#4351,#4352,#2784,.T.);
#5235=EDGE_CURVE('',#4352,#4352,#3748,.T.);
#5236=EDGE_CURVE('',#4353,#4353,#3749,.T.);
#5237=EDGE_CURVE('',#4353,#4354,#2785,.T.);
#5238=EDGE_CURVE('',#4354,#4354,#3750,.T.);
#5239=EDGE_CURVE('',#4355,#4355,#3751,.T.);
#5240=EDGE_CURVE('',#4355,#4356,#2786,.T.);
#5241=EDGE_CURVE('',#4356,#4356,#3752,.T.);
#5242=EDGE_CURVE('',#4357,#4357,#3753,.T.);
#5243=EDGE_CURVE('',#4357,#4358,#2787,.T.);
#5244=EDGE_CURVE('',#4358,#4358,#3754,.T.);
#5245=EDGE_CURVE('',#4359,#4359,#3755,.T.);
#5246=EDGE_CURVE('',#4359,#4360,#2788,.T.);
#5247=EDGE_CURVE('',#4360,#4360,#3756,.T.);
#5248=EDGE_CURVE('',#4361,#4361,#3757,.T.);
#5249=EDGE_CURVE('',#4361,#4362,#2789,.T.);
#5250=EDGE_CURVE('',#4362,#4362,#3758,.T.);
#5251=EDGE_CURVE('',#4363,#4363,#3759,.T.);
#5252=EDGE_CURVE('',#4363,#4364,#2790,.T.);
#5253=EDGE_CURVE('',#4364,#4364,#3760,.T.);
#5254=EDGE_CURVE('',#4365,#4365,#3761,.T.);
#5255=EDGE_CURVE('',#4365,#4366,#2791,.T.);
#5256=EDGE_CURVE('',#4366,#4366,#3762,.T.);
#5257=EDGE_CURVE('',#4367,#4367,#3763,.T.);
#5258=EDGE_CURVE('',#4367,#4368,#2792,.T.);
#5259=EDGE_CURVE('',#4368,#4368,#3764,.T.);
#5260=EDGE_CURVE('',#4369,#4369,#3765,.T.);
#5261=EDGE_CURVE('',#4369,#4370,#2793,.T.);
#5262=EDGE_CURVE('',#4370,#4370,#3766,.T.);
#5263=EDGE_CURVE('',#4371,#4372,#2794,.T.);
#5264=EDGE_CURVE('',#4371,#4373,#2795,.T.);
#5265=EDGE_CURVE('',#4374,#4373,#2796,.T.);
#5266=EDGE_CURVE('',#4372,#4374,#2797,.T.);
#5267=EDGE_CURVE('',#4375,#4376,#2798,.T.);
#5268=EDGE_CURVE('',#4377,#4375,#2799,.T.);
#5269=EDGE_CURVE('',#4378,#4377,#2800,.T.);
#5270=EDGE_CURVE('',#4376,#4378,#2801,.T.);
#5271=EDGE_CURVE('',#4376,#4371,#2802,.T.);
#5272=EDGE_CURVE('',#4373,#4378,#2803,.T.);
#5273=EDGE_CURVE('',#4374,#4377,#2804,.T.);
#5274=EDGE_CURVE('',#4375,#4372,#2805,.T.);
#5275=EDGE_CURVE('',#4379,#4380,#2806,.T.);
#5276=EDGE_CURVE('',#4379,#4381,#2807,.T.);
#5277=EDGE_CURVE('',#4382,#4381,#2808,.T.);
#5278=EDGE_CURVE('',#4380,#4382,#2809,.T.);
#5279=EDGE_CURVE('',#4383,#4384,#2810,.T.);
#5280=EDGE_CURVE('',#4385,#4383,#2811,.T.);
#5281=EDGE_CURVE('',#4386,#4385,#2812,.T.);
#5282=EDGE_CURVE('',#4384,#4386,#2813,.T.);
#5283=EDGE_CURVE('',#4384,#4379,#2814,.T.);
#5284=EDGE_CURVE('',#4381,#4386,#2815,.T.);
#5285=EDGE_CURVE('',#4382,#4385,#2816,.T.);
#5286=EDGE_CURVE('',#4383,#4380,#2817,.T.);
#5287=EDGE_CURVE('',#4387,#4388,#2818,.T.);
#5288=EDGE_CURVE('',#4388,#4389,#2819,.T.);
#5289=EDGE_CURVE('',#4390,#4389,#2820,.T.);
#5290=EDGE_CURVE('',#4387,#4390,#2821,.T.);
#5291=EDGE_CURVE('',#4391,#4387,#2822,.T.);
#5292=EDGE_CURVE('',#4392,#4390,#2823,.T.);
#5293=EDGE_CURVE('',#4391,#4392,#2824,.T.);
#5294=EDGE_CURVE('',#4393,#4391,#2825,.T.);
#5295=EDGE_CURVE('',#4394,#4392,#2826,.T.);
#5296=EDGE_CURVE('',#4393,#4394,#2827,.T.);
#5297=EDGE_CURVE('',#4388,#4393,#2828,.T.);
#5298=EDGE_CURVE('',#4389,#4394,#2829,.T.);
#5299=EDGE_CURVE('',#4395,#4395,#3767,.T.);
#5300=EDGE_CURVE('',#4395,#4396,#2830,.T.);
#5301=EDGE_CURVE('',#4396,#4396,#3768,.T.);
#5302=EDGE_CURVE('',#4397,#4397,#3769,.T.);
#5303=EDGE_CURVE('',#4398,#4398,#3770,.T.);
#5304=EDGE_CURVE('',#4397,#4399,#2831,.T.);
#5305=EDGE_CURVE('',#4399,#4399,#3771,.T.);
#5306=EDGE_CURVE('',#4400,#4400,#3772,.T.);
#5307=EDGE_CURVE('',#4400,#4398,#2832,.T.);
#5308=EDGE_CURVE('',#4401,#4401,#3773,.T.);
#5309=EDGE_CURVE('',#4401,#4402,#2833,.T.);
#5310=EDGE_CURVE('',#4402,#4402,#3774,.T.);
#5311=EDGE_CURVE('',#4403,#4403,#3775,.T.);
#5312=EDGE_CURVE('',#4403,#4404,#2834,.T.);
#5313=EDGE_CURVE('',#4404,#4404,#3776,.T.);
#5314=EDGE_CURVE('',#4405,#4405,#3777,.T.);
#5315=EDGE_CURVE('',#4405,#4406,#2835,.T.);
#5316=EDGE_CURVE('',#4406,#4406,#3778,.T.);
#5317=EDGE_CURVE('',#4407,#4407,#3779,.T.);
#5318=EDGE_CURVE('',#4407,#4408,#2836,.T.);
#5319=EDGE_CURVE('',#4408,#4408,#3780,.T.);
#5320=EDGE_CURVE('',#4409,#4409,#3781,.T.);
#5321=EDGE_CURVE('',#4409,#4410,#2837,.T.);
#5322=EDGE_CURVE('',#4410,#4410,#3782,.T.);
#5323=EDGE_CURVE('',#4411,#4411,#3783,.T.);
#5324=EDGE_CURVE('',#4411,#4412,#2838,.T.);
#5325=EDGE_CURVE('',#4412,#4412,#3784,.T.);
#5326=EDGE_CURVE('',#4413,#4413,#3785,.T.);
#5327=EDGE_CURVE('',#4413,#4414,#2839,.T.);
#5328=EDGE_CURVE('',#4414,#4414,#3786,.T.);
#5329=EDGE_CURVE('',#4415,#4415,#3787,.T.);
#5330=EDGE_CURVE('',#4415,#4416,#2840,.T.);
#5331=EDGE_CURVE('',#4416,#4416,#3788,.T.);
#5332=EDGE_CURVE('',#4417,#4417,#3789,.T.);
#5333=EDGE_CURVE('',#4417,#4418,#2841,.T.);
#5334=EDGE_CURVE('',#4418,#4418,#3790,.T.);
#5335=EDGE_CURVE('',#4419,#4419,#3791,.T.);
#5336=EDGE_CURVE('',#4419,#4420,#2842,.T.);
#5337=EDGE_CURVE('',#4420,#4420,#3792,.T.);
#5338=EDGE_CURVE('',#4421,#4421,#3793,.T.);
#5339=EDGE_CURVE('',#4421,#4422,#2843,.T.);
#5340=EDGE_CURVE('',#4422,#4422,#3794,.T.);
#5341=EDGE_CURVE('',#4423,#4423,#3795,.T.);
#5342=EDGE_CURVE('',#4423,#4424,#2844,.T.);
#5343=EDGE_CURVE('',#4424,#4424,#3796,.T.);
#5344=EDGE_CURVE('',#4425,#4426,#2845,.T.);
#5345=EDGE_CURVE('',#4425,#4427,#2846,.T.);
#5346=EDGE_CURVE('',#4428,#4427,#2847,.T.);
#5347=EDGE_CURVE('',#4426,#4428,#2848,.T.);
#5348=EDGE_CURVE('',#4429,#4430,#2849,.T.);
#5349=EDGE_CURVE('',#4431,#4429,#2850,.T.);
#5350=EDGE_CURVE('',#4432,#4431,#2851,.T.);
#5351=EDGE_CURVE('',#4430,#4432,#2852,.T.);
#5352=EDGE_CURVE('',#4430,#4425,#2853,.T.);
#5353=EDGE_CURVE('',#4427,#4432,#2854,.T.);
#5354=EDGE_CURVE('',#4428,#4431,#2855,.T.);
#5355=EDGE_CURVE('',#4429,#4426,#2856,.T.);
#5356=EDGE_CURVE('',#4433,#4434,#2857,.T.);
#5357=EDGE_CURVE('',#4433,#4435,#2858,.T.);
#5358=EDGE_CURVE('',#4436,#4435,#2859,.T.);
#5359=EDGE_CURVE('',#4434,#4436,#2860,.T.);
#5360=EDGE_CURVE('',#4437,#4438,#2861,.T.);
#5361=EDGE_CURVE('',#4439,#4437,#2862,.T.);
#5362=EDGE_CURVE('',#4440,#4439,#2863,.T.);
#5363=EDGE_CURVE('',#4438,#4440,#2864,.T.);
#5364=EDGE_CURVE('',#4438,#4433,#2865,.T.);
#5365=EDGE_CURVE('',#4435,#4440,#2866,.T.);
#5366=EDGE_CURVE('',#4436,#4439,#2867,.T.);
#5367=EDGE_CURVE('',#4437,#4434,#2868,.T.);
#5368=EDGE_CURVE('',#4441,#4442,#2869,.T.);
#5369=EDGE_CURVE('',#4442,#4443,#2870,.T.);
#5370=EDGE_CURVE('',#4444,#4443,#2871,.T.);
#5371=EDGE_CURVE('',#4441,#4444,#2872,.T.);
#5372=EDGE_CURVE('',#4445,#4441,#2873,.T.);
#5373=EDGE_CURVE('',#4446,#4444,#2874,.T.);
#5374=EDGE_CURVE('',#4445,#4446,#2875,.T.);
#5375=EDGE_CURVE('',#4447,#4445,#2876,.T.);
#5376=EDGE_CURVE('',#4448,#4446,#2877,.T.);
#5377=EDGE_CURVE('',#4447,#4448,#2878,.T.);
#5378=EDGE_CURVE('',#4442,#4447,#2879,.T.);
#5379=EDGE_CURVE('',#4443,#4448,#2880,.T.);
#5380=EDGE_CURVE('',#4449,#4449,#3797,.T.);
#5381=EDGE_CURVE('',#4449,#4450,#2881,.T.);
#5382=EDGE_CURVE('',#4450,#4450,#3798,.T.);
#5383=EDGE_CURVE('',#4451,#4451,#3799,.T.);
#5384=EDGE_CURVE('',#4452,#4452,#3800,.T.);
#5385=EDGE_CURVE('',#4451,#4453,#2882,.T.);
#5386=EDGE_CURVE('',#4453,#4453,#3801,.T.);
#5387=EDGE_CURVE('',#4454,#4454,#3802,.T.);
#5388=EDGE_CURVE('',#4454,#4452,#2883,.T.);
#5389=EDGE_CURVE('',#4455,#4455,#3803,.T.);
#5390=EDGE_CURVE('',#4455,#4456,#2884,.T.);
#5391=EDGE_CURVE('',#4456,#4456,#3804,.T.);
#5392=EDGE_CURVE('',#4457,#4457,#3805,.T.);
#5393=EDGE_CURVE('',#4457,#4458,#2885,.T.);
#5394=EDGE_CURVE('',#4458,#4458,#3806,.T.);
#5395=EDGE_CURVE('',#4459,#4459,#3807,.T.);
#5396=EDGE_CURVE('',#4459,#4460,#2886,.T.);
#5397=EDGE_CURVE('',#4460,#4460,#3808,.T.);
#5398=EDGE_CURVE('',#4461,#4461,#3809,.T.);
#5399=EDGE_CURVE('',#4461,#4462,#2887,.T.);
#5400=EDGE_CURVE('',#4462,#4462,#3810,.T.);
#5401=EDGE_CURVE('',#4463,#4463,#3811,.T.);
#5402=EDGE_CURVE('',#4463,#4464,#2888,.T.);
#5403=EDGE_CURVE('',#4464,#4464,#3812,.T.);
#5404=EDGE_CURVE('',#4465,#4465,#3813,.T.);
#5405=EDGE_CURVE('',#4465,#4466,#2889,.T.);
#5406=EDGE_CURVE('',#4466,#4466,#3814,.T.);
#5407=EDGE_CURVE('',#4467,#4468,#2890,.T.);
#5408=EDGE_CURVE('',#4468,#4469,#2891,.T.);
#5409=EDGE_CURVE('',#4469,#4470,#2892,.T.);
#5410=EDGE_CURVE('',#4467,#4470,#2893,.T.);
#5411=EDGE_CURVE('',#4468,#4471,#2894,.T.);
#5412=EDGE_CURVE('',#4471,#4472,#2895,.T.);
#5413=EDGE_CURVE('',#4472,#4469,#2896,.T.);
#5414=EDGE_CURVE('',#4471,#4473,#2897,.T.);
#5415=EDGE_CURVE('',#4473,#4474,#2898,.T.);
#5416=EDGE_CURVE('',#4474,#4472,#2899,.T.);
#5417=EDGE_CURVE('',#4473,#4475,#2900,.T.);
#5418=EDGE_CURVE('',#4475,#4476,#2901,.T.);
#5419=EDGE_CURVE('',#4476,#4474,#2902,.T.);
#5420=EDGE_CURVE('',#4475,#4477,#2903,.T.);
#5421=EDGE_CURVE('',#4477,#4478,#2904,.T.);
#5422=EDGE_CURVE('',#4478,#4476,#2905,.T.);
#5423=EDGE_CURVE('',#4477,#4467,#2906,.T.);
#5424=EDGE_CURVE('',#4470,#4478,#2907,.T.);
#5425=EDGE_CURVE('',#4479,#4479,#3815,.T.);
#5426=EDGE_CURVE('',#4480,#4480,#3816,.T.);
#5427=EDGE_CURVE('',#4481,#4481,#3817,.T.);
#5428=EDGE_CURVE('',#4481,#4480,#2908,.T.);
#5429=EDGE_CURVE('',#4482,#4482,#3818,.T.);
#5430=EDGE_CURVE('',#4482,#4481,#2909,.T.);
#5431=EDGE_CURVE('',#4483,#4483,#3819,.T.);
#5432=EDGE_CURVE('',#4483,#4482,#2910,.T.);
#5433=EDGE_CURVE('',#4484,#4484,#3820,.T.);
#5434=EDGE_CURVE('',#4485,#4485,#3821,.F.);
#5435=EDGE_CURVE('',#4485,#4484,#2911,.T.);
#5436=EDGE_CURVE('',#4479,#4485,#2912,.T.);
#5437=EDGE_CURVE('',#4486,#4487,#2913,.T.);
#5438=EDGE_CURVE('',#4487,#4488,#2914,.T.);
#5439=EDGE_CURVE('',#4488,#4489,#2915,.T.);
#5440=EDGE_CURVE('',#4486,#4489,#2916,.T.);
#5441=EDGE_CURVE('',#4487,#4490,#2917,.T.);
#5442=EDGE_CURVE('',#4490,#4491,#2918,.T.);
#5443=EDGE_CURVE('',#4491,#4488,#2919,.T.);
#5444=EDGE_CURVE('',#4490,#4492,#2920,.T.);
#5445=EDGE_CURVE('',#4492,#4493,#2921,.T.);
#5446=EDGE_CURVE('',#4493,#4491,#2922,.T.);
#5447=EDGE_CURVE('',#4492,#4494,#2923,.T.);
#5448=EDGE_CURVE('',#4494,#4495,#2924,.T.);
#5449=EDGE_CURVE('',#4495,#4493,#2925,.T.);
#5450=EDGE_CURVE('',#4494,#4496,#2926,.T.);
#5451=EDGE_CURVE('',#4496,#4497,#2927,.T.);
#5452=EDGE_CURVE('',#4497,#4495,#2928,.T.);
#5453=EDGE_CURVE('',#4496,#4486,#2929,.T.);
#5454=EDGE_CURVE('',#4489,#4497,#2930,.T.);
#5455=EDGE_CURVE('',#4498,#4498,#3822,.T.);
#5456=EDGE_CURVE('',#4499,#4499,#3823,.T.);
#5457=EDGE_CURVE('',#4500,#4500,#3824,.T.);
#5458=EDGE_CURVE('',#4500,#4499,#2931,.T.);
#5459=EDGE_CURVE('',#4501,#4501,#3825,.T.);
#5460=EDGE_CURVE('',#4501,#4500,#2932,.T.);
#5461=EDGE_CURVE('',#4502,#4502,#3826,.T.);
#5462=EDGE_CURVE('',#4502,#4501,#2933,.T.);
#5463=EDGE_CURVE('',#4503,#4503,#3827,.T.);
#5464=EDGE_CURVE('',#4504,#4504,#3828,.F.);
#5465=EDGE_CURVE('',#4504,#4503,#2934,.T.);
#5466=EDGE_CURVE('',#4498,#4504,#2935,.T.);
#5467=EDGE_CURVE('',#4505,#4505,#3829,.T.);
#5468=EDGE_CURVE('',#4505,#4506,#2936,.T.);
#5469=EDGE_CURVE('',#4506,#4506,#3830,.T.);
#5470=EDGE_CURVE('',#4507,#4507,#3831,.T.);
#5471=EDGE_CURVE('',#4507,#4508,#2937,.T.);
#5472=EDGE_CURVE('',#4508,#4508,#3832,.T.);
#5473=EDGE_CURVE('',#4509,#4509,#3833,.T.);
#5474=EDGE_CURVE('',#4509,#4510,#2938,.T.);
#5475=EDGE_CURVE('',#4510,#4510,#3834,.T.);
#5476=EDGE_CURVE('',#4511,#4511,#3835,.T.);
#5477=EDGE_CURVE('',#4511,#4512,#2939,.T.);
#5478=EDGE_CURVE('',#4512,#4512,#3836,.T.);
#5479=EDGE_CURVE('',#4513,#4513,#3837,.T.);
#5480=EDGE_CURVE('',#4513,#4514,#2940,.T.);
#5481=EDGE_CURVE('',#4514,#4514,#3838,.T.);
#5482=EDGE_CURVE('',#4515,#4515,#3839,.T.);
#5483=EDGE_CURVE('',#4515,#4516,#2941,.T.);
#5484=EDGE_CURVE('',#4516,#4516,#3840,.T.);
#5485=EDGE_CURVE('',#4517,#4517,#3841,.T.);
#5486=EDGE_CURVE('',#4517,#4518,#2942,.T.);
#5487=EDGE_CURVE('',#4518,#4518,#3842,.T.);
#5488=EDGE_CURVE('',#4519,#4519,#3843,.T.);
#5489=EDGE_CURVE('',#4519,#4520,#2943,.T.);
#5490=EDGE_CURVE('',#4520,#4520,#3844,.T.);
#5491=EDGE_CURVE('',#4521,#4521,#3845,.T.);
#5492=EDGE_CURVE('',#4521,#4522,#2944,.T.);
#5493=EDGE_CURVE('',#4522,#4522,#3846,.T.);
#5494=EDGE_CURVE('',#4523,#4523,#3847,.T.);
#5495=EDGE_CURVE('',#4523,#4524,#2945,.T.);
#5496=EDGE_CURVE('',#4524,#4524,#3848,.T.);
#5497=EDGE_CURVE('',#4525,#4525,#3849,.T.);
#5498=EDGE_CURVE('',#4525,#4526,#2946,.T.);
#5499=EDGE_CURVE('',#4526,#4526,#3850,.T.);
#5500=EDGE_CURVE('',#4527,#4527,#3851,.T.);
#5501=EDGE_CURVE('',#4527,#4528,#2947,.T.);
#5502=EDGE_CURVE('',#4528,#4528,#3852,.T.);
#5503=EDGE_CURVE('',#4529,#4529,#3853,.T.);
#5504=EDGE_CURVE('',#4529,#4530,#2948,.T.);
#5505=EDGE_CURVE('',#4530,#4530,#3854,.T.);
#5506=EDGE_CURVE('',#4531,#4531,#3855,.T.);
#5507=EDGE_CURVE('',#4531,#4532,#2949,.T.);
#5508=EDGE_CURVE('',#4532,#4532,#3856,.T.);
#5509=EDGE_CURVE('',#4533,#4533,#3857,.T.);
#5510=EDGE_CURVE('',#4533,#4534,#2950,.T.);
#5511=EDGE_CURVE('',#4534,#4534,#3858,.T.);
#5512=EDGE_CURVE('',#4535,#4535,#3859,.T.);
#5513=EDGE_CURVE('',#4535,#4536,#2951,.T.);
#5514=EDGE_CURVE('',#4536,#4536,#3860,.T.);
#5515=EDGE_CURVE('',#4537,#4537,#3861,.T.);
#5516=EDGE_CURVE('',#4537,#4538,#2952,.T.);
#5517=EDGE_CURVE('',#4538,#4538,#3862,.T.);
#5518=EDGE_CURVE('',#4539,#4539,#3863,.T.);
#5519=EDGE_CURVE('',#4539,#4540,#2953,.T.);
#5520=EDGE_CURVE('',#4540,#4540,#3864,.T.);
#5521=EDGE_CURVE('',#4541,#4541,#3865,.T.);
#5522=EDGE_CURVE('',#4541,#4542,#2954,.T.);
#5523=EDGE_CURVE('',#4542,#4542,#3866,.T.);
#5524=EDGE_CURVE('',#4543,#4543,#3867,.T.);
#5525=EDGE_CURVE('',#4543,#4544,#2955,.T.);
#5526=EDGE_CURVE('',#4544,#4544,#3868,.T.);
#5527=EDGE_CURVE('',#4545,#4545,#3869,.T.);
#5528=EDGE_CURVE('',#4545,#4546,#2956,.T.);
#5529=EDGE_CURVE('',#4546,#4546,#3870,.T.);
#5530=EDGE_CURVE('',#4547,#4547,#3871,.T.);
#5531=EDGE_CURVE('',#4547,#4548,#2957,.T.);
#5532=EDGE_CURVE('',#4548,#4548,#3872,.T.);
#5533=EDGE_CURVE('',#4549,#4549,#3873,.T.);
#5534=EDGE_CURVE('',#4549,#4550,#2958,.T.);
#5535=EDGE_CURVE('',#4550,#4550,#3874,.T.);
#5536=EDGE_CURVE('',#4551,#4551,#3875,.T.);
#5537=EDGE_CURVE('',#4551,#4552,#2959,.T.);
#5538=EDGE_CURVE('',#4552,#4552,#3876,.T.);
#5539=EDGE_CURVE('',#4553,#4554,#3877,.T.);
#5540=EDGE_CURVE('',#4554,#4553,#3878,.T.);
#5541=EDGE_CURVE('',#4554,#4555,#3879,.T.);
#5542=EDGE_CURVE('',#4556,#4555,#3880,.T.);
#5543=EDGE_CURVE('',#4555,#4556,#3881,.T.);
#5544=EDGE_CURVE('',#4556,#4557,#2960,.T.);
#5545=EDGE_CURVE('',#4557,#4557,#3882,.T.);
#5546=EDGE_CURVE('',#4558,#4558,#3883,.T.);
#5547=EDGE_CURVE('',#4558,#4559,#2961,.T.);
#5548=EDGE_CURVE('',#4559,#4559,#3884,.T.);
#5549=EDGE_CURVE('',#4559,#4560,#2962,.T.);
#5550=EDGE_CURVE('',#4560,#4560,#3885,.T.);
#5551=EDGE_CURVE('',#4561,#4561,#3886,.T.);
#5552=EDGE_CURVE('',#4561,#4553,#2963,.T.);
#5553=EDGE_CURVE('',#4562,#4562,#3887,.T.);
#5554=EDGE_CURVE('',#4562,#4558,#2964,.T.);
#5555=EDGE_CURVE('',#4563,#4564,#3888,.T.);
#5556=EDGE_CURVE('',#4564,#4563,#3889,.T.);
#5557=EDGE_CURVE('',#4564,#4565,#3890,.T.);
#5558=EDGE_CURVE('',#4566,#4565,#3891,.T.);
#5559=EDGE_CURVE('',#4565,#4566,#3892,.T.);
#5560=EDGE_CURVE('',#4567,#4567,#3893,.T.);
#5561=EDGE_CURVE('',#4567,#4566,#2965,.T.);
#5562=EDGE_CURVE('',#4568,#4568,#3894,.T.);
#5563=EDGE_CURVE('',#4569,#4569,#3895,.T.);
#5564=EDGE_CURVE('',#4570,#4570,#3896,.T.);
#5565=EDGE_CURVE('',#4570,#4568,#2966,.T.);
#5566=EDGE_CURVE('',#4571,#4571,#3897,.T.);
#5567=EDGE_CURVE('',#4571,#4570,#2967,.T.);
#5568=EDGE_CURVE('',#4572,#4572,#3898,.T.);
#5569=EDGE_CURVE('',#4572,#4571,#2968,.T.);
#5570=EDGE_CURVE('',#4563,#4569,#2969,.T.);
#5571=EDGE_CURVE('',#4573,#4574,#3899,.T.);
#5572=EDGE_CURVE('',#4575,#4576,#3900,.T.);
#5573=EDGE_CURVE('',#4577,#4578,#3901,.T.);
#5574=EDGE_CURVE('',#4579,#4580,#3902,.T.);
#5575=EDGE_CURVE('',#4581,#4582,#3903,.T.);
#5576=EDGE_CURVE('',#4583,#4584,#3904,.T.);
#5577=EDGE_CURVE('',#4585,#4586,#3905,.T.);
#5578=EDGE_CURVE('',#4587,#4588,#3906,.T.);
#5579=EDGE_CURVE('',#4589,#4590,#420,.T.);
#5580=EDGE_CURVE('',#4591,#4589,#3907,.T.);
#5581=EDGE_CURVE('',#4592,#4591,#421,.T.);
#5582=EDGE_CURVE('',#4590,#4592,#3908,.T.);
#5583=EDGE_CURVE('',#4593,#4591,#3909,.T.);
#5584=EDGE_CURVE('',#4593,#4594,#422,.T.);
#5585=EDGE_CURVE('',#4595,#4594,#3910,.T.);
#5586=EDGE_CURVE('',#4595,#4596,#423,.T.);
#5587=EDGE_CURVE('',#4597,#4596,#3911,.T.);
#5588=EDGE_CURVE('',#4597,#4598,#424,.T.);
#5589=EDGE_CURVE('',#4598,#4599,#2970,.T.);
#5590=EDGE_CURVE('',#4599,#4599,#3912,.T.);
#5591=EDGE_CURVE('',#4598,#4600,#425,.T.);
#5592=EDGE_CURVE('',#4601,#4600,#3913,.T.);
#5593=EDGE_CURVE('',#4601,#4602,#426,.T.);
#5594=EDGE_CURVE('',#4603,#4602,#3914,.T.);
#5595=EDGE_CURVE('',#4603,#4604,#427,.T.);
#5596=EDGE_CURVE('',#4605,#4604,#3915,.T.);
#5597=EDGE_CURVE('',#4605,#4606,#428,.T.);
#5598=EDGE_CURVE('',#4607,#4606,#3916,.T.);
#5599=EDGE_CURVE('',#4607,#4608,#429,.T.);
#5600=EDGE_CURVE('',#4592,#4608,#3917,.T.);
#5601=EDGE_CURVE('',#4589,#4609,#3918,.T.);
#5602=EDGE_CURVE('',#4609,#4593,#3919,.T.);
#5603=EDGE_CURVE('',#4610,#4609,#430,.T.);
#5604=EDGE_CURVE('',#4594,#4610,#3920,.T.);
#5605=EDGE_CURVE('',#4610,#4611,#3921,.T.);
#5606=EDGE_CURVE('',#4611,#4595,#3922,.T.);
#5607=EDGE_CURVE('',#4612,#4611,#431,.T.);
#5608=EDGE_CURVE('',#4596,#4612,#3923,.T.);
#5609=EDGE_CURVE('',#4612,#4613,#3924,.T.);
#5610=EDGE_CURVE('',#4613,#4597,#3925,.T.);
#5611=EDGE_CURVE('',#4614,#4615,#432,.T.);
#5612=EDGE_CURVE('',#4600,#4614,#3926,.T.);
#5613=EDGE_CURVE('',#4615,#4613,#433,.T.);
#5614=EDGE_CURVE('',#4614,#4616,#3927,.T.);
#5615=EDGE_CURVE('',#4616,#4601,#3928,.T.);
#5616=EDGE_CURVE('',#4617,#4616,#434,.T.);
#5617=EDGE_CURVE('',#4602,#4617,#3929,.T.);
#5618=EDGE_CURVE('',#4617,#4618,#3930,.T.);
#5619=EDGE_CURVE('',#4618,#4603,#3931,.T.);
#5620=EDGE_CURVE('',#4619,#4618,#435,.T.);
#5621=EDGE_CURVE('',#4604,#4619,#3932,.T.);
#5622=EDGE_CURVE('',#4619,#4620,#3933,.T.);
#5623=EDGE_CURVE('',#4620,#4605,#3934,.T.);
#5624=EDGE_CURVE('',#4621,#4620,#436,.T.);
#5625=EDGE_CURVE('',#4606,#4621,#3935,.T.);
#5626=EDGE_CURVE('',#4622,#4622,#3936,.T.);
#5627=EDGE_CURVE('',#4622,#4615,#2971,.T.);
#5628=EDGE_CURVE('',#4623,#4590,#3937,.T.);
#5629=EDGE_CURVE('',#4623,#4624,#437,.T.);
#5630=EDGE_CURVE('',#4621,#4624,#3938,.T.);
#5631=EDGE_CURVE('',#4608,#4623,#3939,.T.);
#5632=EDGE_CURVE('',#4624,#4607,#3940,.T.);
#5633=EDGE_CURVE('',#4625,#4625,#3941,.T.);
#5634=EDGE_CURVE('',#4626,#4626,#3942,.T.);
#5635=EDGE_CURVE('',#4627,#4627,#3943,.T.);
#5636=EDGE_CURVE('',#4627,#4625,#2972,.T.);
#5637=EDGE_CURVE('',#4628,#4628,#3944,.T.);
#5638=EDGE_CURVE('',#4628,#4626,#2973,.T.);
#5639=EDGE_CURVE('',#4629,#4629,#3945,.T.);
#5640=EDGE_CURVE('',#4630,#4630,#3946,.T.);
#5641=EDGE_CURVE('',#4631,#4631,#3947,.T.);
#5642=EDGE_CURVE('',#4631,#4629,#2974,.T.);
#5643=EDGE_CURVE('',#4632,#4632,#3948,.T.);
#5644=EDGE_CURVE('',#4632,#4630,#2975,.T.);
#5645=ORIENTED_EDGE('',*,*,#4633,.F.);
#5646=ORIENTED_EDGE('',*,*,#4634,.T.);
#5647=ORIENTED_EDGE('',*,*,#4635,.F.);
#5648=ORIENTED_EDGE('',*,*,#4634,.F.);
#5649=ORIENTED_EDGE('',*,*,#4636,.F.);
#5650=ORIENTED_EDGE('',*,*,#4637,.T.);
#5651=ORIENTED_EDGE('',*,*,#4638,.F.);
#5652=ORIENTED_EDGE('',*,*,#4637,.F.);
#5653=ORIENTED_EDGE('',*,*,#4639,.F.);
#5654=ORIENTED_EDGE('',*,*,#4640,.T.);
#5655=ORIENTED_EDGE('',*,*,#4641,.F.);
#5656=ORIENTED_EDGE('',*,*,#4640,.F.);
#5657=ORIENTED_EDGE('',*,*,#4642,.F.);
#5658=ORIENTED_EDGE('',*,*,#4643,.T.);
#5659=ORIENTED_EDGE('',*,*,#4644,.F.);
#5660=ORIENTED_EDGE('',*,*,#4643,.F.);
#5661=ORIENTED_EDGE('',*,*,#4645,.F.);
#5662=ORIENTED_EDGE('',*,*,#4646,.T.);
#5663=ORIENTED_EDGE('',*,*,#4647,.F.);
#5664=ORIENTED_EDGE('',*,*,#4646,.F.);
#5665=ORIENTED_EDGE('',*,*,#4648,.F.);
#5666=ORIENTED_EDGE('',*,*,#4649,.T.);
#5667=ORIENTED_EDGE('',*,*,#4650,.F.);
#5668=ORIENTED_EDGE('',*,*,#4649,.F.);
#5669=ORIENTED_EDGE('',*,*,#4651,.F.);
#5670=ORIENTED_EDGE('',*,*,#4652,.T.);
#5671=ORIENTED_EDGE('',*,*,#4653,.F.);
#5672=ORIENTED_EDGE('',*,*,#4652,.F.);
#5673=ORIENTED_EDGE('',*,*,#4654,.F.);
#5674=ORIENTED_EDGE('',*,*,#4655,.T.);
#5675=ORIENTED_EDGE('',*,*,#4656,.F.);
#5676=ORIENTED_EDGE('',*,*,#4655,.F.);
#5677=ORIENTED_EDGE('',*,*,#4657,.F.);
#5678=ORIENTED_EDGE('',*,*,#4658,.T.);
#5679=ORIENTED_EDGE('',*,*,#4659,.F.);
#5680=ORIENTED_EDGE('',*,*,#4658,.F.);
#5681=ORIENTED_EDGE('',*,*,#4660,.F.);
#5682=ORIENTED_EDGE('',*,*,#4661,.T.);
#5683=ORIENTED_EDGE('',*,*,#4662,.F.);
#5684=ORIENTED_EDGE('',*,*,#4661,.F.);
#5685=ORIENTED_EDGE('',*,*,#4663,.F.);
#5686=ORIENTED_EDGE('',*,*,#4664,.T.);
#5687=ORIENTED_EDGE('',*,*,#4665,.F.);
#5688=ORIENTED_EDGE('',*,*,#4664,.F.);
#5689=ORIENTED_EDGE('',*,*,#4666,.F.);
#5690=ORIENTED_EDGE('',*,*,#4667,.T.);
#5691=ORIENTED_EDGE('',*,*,#4668,.F.);
#5692=ORIENTED_EDGE('',*,*,#4667,.F.);
#5693=ORIENTED_EDGE('',*,*,#4669,.F.);
#5694=ORIENTED_EDGE('',*,*,#4670,.T.);
#5695=ORIENTED_EDGE('',*,*,#4671,.F.);
#5696=ORIENTED_EDGE('',*,*,#4670,.F.);
#5697=ORIENTED_EDGE('',*,*,#4672,.F.);
#5698=ORIENTED_EDGE('',*,*,#4673,.T.);
#5699=ORIENTED_EDGE('',*,*,#4674,.F.);
#5700=ORIENTED_EDGE('',*,*,#4673,.F.);
#5701=ORIENTED_EDGE('',*,*,#4675,.F.);
#5702=ORIENTED_EDGE('',*,*,#4676,.T.);
#5703=ORIENTED_EDGE('',*,*,#4677,.F.);
#5704=ORIENTED_EDGE('',*,*,#4676,.F.);
#5705=ORIENTED_EDGE('',*,*,#4678,.F.);
#5706=ORIENTED_EDGE('',*,*,#4679,.T.);
#5707=ORIENTED_EDGE('',*,*,#4680,.F.);
#5708=ORIENTED_EDGE('',*,*,#4679,.F.);
#5709=ORIENTED_EDGE('',*,*,#4681,.F.);
#5710=ORIENTED_EDGE('',*,*,#4682,.T.);
#5711=ORIENTED_EDGE('',*,*,#4683,.F.);
#5712=ORIENTED_EDGE('',*,*,#4682,.F.);
#5713=ORIENTED_EDGE('',*,*,#4684,.F.);
#5714=ORIENTED_EDGE('',*,*,#4685,.T.);
#5715=ORIENTED_EDGE('',*,*,#4686,.F.);
#5716=ORIENTED_EDGE('',*,*,#4685,.F.);
#5717=ORIENTED_EDGE('',*,*,#4687,.F.);
#5718=ORIENTED_EDGE('',*,*,#4688,.T.);
#5719=ORIENTED_EDGE('',*,*,#4689,.F.);
#5720=ORIENTED_EDGE('',*,*,#4688,.F.);
#5721=ORIENTED_EDGE('',*,*,#4690,.F.);
#5722=ORIENTED_EDGE('',*,*,#4691,.T.);
#5723=ORIENTED_EDGE('',*,*,#4692,.F.);
#5724=ORIENTED_EDGE('',*,*,#4691,.F.);
#5725=ORIENTED_EDGE('',*,*,#4693,.T.);
#5726=ORIENTED_EDGE('',*,*,#4694,.T.);
#5727=ORIENTED_EDGE('',*,*,#4695,.F.);
#5728=ORIENTED_EDGE('',*,*,#4696,.F.);
#5729=ORIENTED_EDGE('',*,*,#4697,.T.);
#5730=ORIENTED_EDGE('',*,*,#4696,.T.);
#5731=ORIENTED_EDGE('',*,*,#4698,.F.);
#5732=ORIENTED_EDGE('',*,*,#4699,.F.);
#5733=ORIENTED_EDGE('',*,*,#4700,.T.);
#5734=ORIENTED_EDGE('',*,*,#4699,.T.);
#5735=ORIENTED_EDGE('',*,*,#4701,.F.);
#5736=ORIENTED_EDGE('',*,*,#4702,.F.);
#5737=ORIENTED_EDGE('',*,*,#4703,.T.);
#5738=ORIENTED_EDGE('',*,*,#4702,.T.);
#5739=ORIENTED_EDGE('',*,*,#4704,.F.);
#5740=ORIENTED_EDGE('',*,*,#4694,.F.);
#5741=ORIENTED_EDGE('',*,*,#4704,.T.);
#5742=ORIENTED_EDGE('',*,*,#4701,.T.);
#5743=ORIENTED_EDGE('',*,*,#4698,.T.);
#5744=ORIENTED_EDGE('',*,*,#4695,.T.);
#5745=ORIENTED_EDGE('',*,*,#4647,.T.);
#5746=ORIENTED_EDGE('',*,*,#4650,.T.);
#5747=ORIENTED_EDGE('',*,*,#4653,.T.);
#5748=ORIENTED_EDGE('',*,*,#4656,.T.);
#5749=ORIENTED_EDGE('',*,*,#4671,.T.);
#5750=ORIENTED_EDGE('',*,*,#4674,.T.);
#5751=ORIENTED_EDGE('',*,*,#4677,.T.);
#5752=ORIENTED_EDGE('',*,*,#4680,.T.);
#5753=ORIENTED_EDGE('',*,*,#4683,.T.);
#5754=ORIENTED_EDGE('',*,*,#4686,.T.);
#5755=ORIENTED_EDGE('',*,*,#4689,.T.);
#5756=ORIENTED_EDGE('',*,*,#4692,.T.);
#5757=ORIENTED_EDGE('',*,*,#4668,.T.);
#5758=ORIENTED_EDGE('',*,*,#4665,.T.);
#5759=ORIENTED_EDGE('',*,*,#4662,.T.);
#5760=ORIENTED_EDGE('',*,*,#4659,.T.);
#5761=ORIENTED_EDGE('',*,*,#4644,.T.);
#5762=ORIENTED_EDGE('',*,*,#4641,.T.);
#5763=ORIENTED_EDGE('',*,*,#4638,.T.);
#5764=ORIENTED_EDGE('',*,*,#4635,.T.);
#5765=ORIENTED_EDGE('',*,*,#4703,.F.);
#5766=ORIENTED_EDGE('',*,*,#4693,.F.);
#5767=ORIENTED_EDGE('',*,*,#4697,.F.);
#5768=ORIENTED_EDGE('',*,*,#4700,.F.);
#5769=ORIENTED_EDGE('',*,*,#4645,.T.);
#5770=ORIENTED_EDGE('',*,*,#4648,.T.);
#5771=ORIENTED_EDGE('',*,*,#4651,.T.);
#5772=ORIENTED_EDGE('',*,*,#4654,.T.);
#5773=ORIENTED_EDGE('',*,*,#4669,.T.);
#5774=ORIENTED_EDGE('',*,*,#4672,.T.);
#5775=ORIENTED_EDGE('',*,*,#4675,.T.);
#5776=ORIENTED_EDGE('',*,*,#4678,.T.);
#5777=ORIENTED_EDGE('',*,*,#4681,.T.);
#5778=ORIENTED_EDGE('',*,*,#4684,.T.);
#5779=ORIENTED_EDGE('',*,*,#4687,.T.);
#5780=ORIENTED_EDGE('',*,*,#4690,.T.);
#5781=ORIENTED_EDGE('',*,*,#4666,.T.);
#5782=ORIENTED_EDGE('',*,*,#4663,.T.);
#5783=ORIENTED_EDGE('',*,*,#4660,.T.);
#5784=ORIENTED_EDGE('',*,*,#4657,.T.);
#5785=ORIENTED_EDGE('',*,*,#4642,.T.);
#5786=ORIENTED_EDGE('',*,*,#4639,.T.);
#5787=ORIENTED_EDGE('',*,*,#4636,.T.);
#5788=ORIENTED_EDGE('',*,*,#4633,.T.);
#5789=ORIENTED_EDGE('',*,*,#4705,.F.);
#5790=ORIENTED_EDGE('',*,*,#4706,.F.);
#5791=ORIENTED_EDGE('',*,*,#4707,.T.);
#5792=ORIENTED_EDGE('',*,*,#4708,.F.);
#5793=ORIENTED_EDGE('',*,*,#4709,.F.);
#5794=ORIENTED_EDGE('',*,*,#4710,.F.);
#5795=ORIENTED_EDGE('',*,*,#4711,.T.);
#5796=ORIENTED_EDGE('',*,*,#4712,.F.);
#5797=ORIENTED_EDGE('',*,*,#4713,.F.);
#5798=ORIENTED_EDGE('',*,*,#4714,.F.);
#5799=ORIENTED_EDGE('',*,*,#4715,.T.);
#5800=ORIENTED_EDGE('',*,*,#4716,.F.);
#5801=ORIENTED_EDGE('',*,*,#4717,.F.);
#5802=ORIENTED_EDGE('',*,*,#4718,.F.);
#5803=ORIENTED_EDGE('',*,*,#4719,.T.);
#5804=ORIENTED_EDGE('',*,*,#4720,.F.);
#5805=ORIENTED_EDGE('',*,*,#4721,.F.);
#5806=ORIENTED_EDGE('',*,*,#4722,.T.);
#5807=ORIENTED_EDGE('',*,*,#4723,.F.);
#5808=ORIENTED_EDGE('',*,*,#4722,.F.);
#5809=ORIENTED_EDGE('',*,*,#4721,.T.);
#5810=ORIENTED_EDGE('',*,*,#4724,.F.);
#5811=ORIENTED_EDGE('',*,*,#4725,.T.);
#5812=ORIENTED_EDGE('',*,*,#4726,.F.);
#5813=ORIENTED_EDGE('',*,*,#4725,.F.);
#5814=ORIENTED_EDGE('',*,*,#4724,.T.);
#5815=ORIENTED_EDGE('',*,*,#4727,.F.);
#5816=ORIENTED_EDGE('',*,*,#4728,.T.);
#5817=ORIENTED_EDGE('',*,*,#4729,.F.);
#5818=ORIENTED_EDGE('',*,*,#4728,.F.);
#5819=ORIENTED_EDGE('',*,*,#4727,.T.);
#5820=ORIENTED_EDGE('',*,*,#4730,.F.);
#5821=ORIENTED_EDGE('',*,*,#4731,.T.);
#5822=ORIENTED_EDGE('',*,*,#4732,.F.);
#5823=ORIENTED_EDGE('',*,*,#4731,.F.);
#5824=ORIENTED_EDGE('',*,*,#4730,.T.);
#5825=ORIENTED_EDGE('',*,*,#4717,.T.);
#5826=ORIENTED_EDGE('',*,*,#4733,.F.);
#5827=ORIENTED_EDGE('',*,*,#4734,.F.);
#5828=ORIENTED_EDGE('',*,*,#4735,.F.);
#5829=ORIENTED_EDGE('',*,*,#4718,.T.);
#5830=ORIENTED_EDGE('',*,*,#4735,.T.);
#5831=ORIENTED_EDGE('',*,*,#4736,.F.);
#5832=ORIENTED_EDGE('',*,*,#4713,.T.);
#5833=ORIENTED_EDGE('',*,*,#4737,.F.);
#5834=ORIENTED_EDGE('',*,*,#4738,.F.);
#5835=ORIENTED_EDGE('',*,*,#4739,.F.);
#5836=ORIENTED_EDGE('',*,*,#4714,.T.);
#5837=ORIENTED_EDGE('',*,*,#4739,.T.);
#5838=ORIENTED_EDGE('',*,*,#4740,.F.);
#5839=ORIENTED_EDGE('',*,*,#4709,.T.);
#5840=ORIENTED_EDGE('',*,*,#4741,.F.);
#5841=ORIENTED_EDGE('',*,*,#4742,.F.);
#5842=ORIENTED_EDGE('',*,*,#4743,.F.);
#5843=ORIENTED_EDGE('',*,*,#4710,.T.);
#5844=ORIENTED_EDGE('',*,*,#4743,.T.);
#5845=ORIENTED_EDGE('',*,*,#4744,.F.);
#5846=ORIENTED_EDGE('',*,*,#4705,.T.);
#5847=ORIENTED_EDGE('',*,*,#4745,.F.);
#5848=ORIENTED_EDGE('',*,*,#4746,.F.);
#5849=ORIENTED_EDGE('',*,*,#4747,.F.);
#5850=ORIENTED_EDGE('',*,*,#4706,.T.);
#5851=ORIENTED_EDGE('',*,*,#4747,.T.);
#5852=ORIENTED_EDGE('',*,*,#4748,.F.);
#5853=ORIENTED_EDGE('',*,*,#4749,.T.);
#5854=ORIENTED_EDGE('',*,*,#4733,.T.);
#5855=ORIENTED_EDGE('',*,*,#4720,.T.);
#5856=ORIENTED_EDGE('',*,*,#4750,.T.);
#5857=ORIENTED_EDGE('',*,*,#4745,.T.);
#5858=ORIENTED_EDGE('',*,*,#4708,.T.);
#5859=ORIENTED_EDGE('',*,*,#4751,.T.);
#5860=ORIENTED_EDGE('',*,*,#4741,.T.);
#5861=ORIENTED_EDGE('',*,*,#4712,.T.);
#5862=ORIENTED_EDGE('',*,*,#4752,.T.);
#5863=ORIENTED_EDGE('',*,*,#4737,.T.);
#5864=ORIENTED_EDGE('',*,*,#4716,.T.);
#5865=ORIENTED_EDGE('',*,*,#4753,.T.);
#5866=ORIENTED_EDGE('',*,*,#4732,.T.);
#5867=ORIENTED_EDGE('',*,*,#4729,.T.);
#5868=ORIENTED_EDGE('',*,*,#4726,.T.);
#5869=ORIENTED_EDGE('',*,*,#4723,.T.);
#5870=ORIENTED_EDGE('',*,*,#4754,.F.);
#5871=ORIENTED_EDGE('',*,*,#4755,.T.);
#5872=ORIENTED_EDGE('',*,*,#4736,.T.);
#5873=ORIENTED_EDGE('',*,*,#4755,.F.);
#5874=ORIENTED_EDGE('',*,*,#4756,.F.);
#5875=ORIENTED_EDGE('',*,*,#4757,.T.);
#5876=ORIENTED_EDGE('',*,*,#4740,.T.);
#5877=ORIENTED_EDGE('',*,*,#4757,.F.);
#5878=ORIENTED_EDGE('',*,*,#4758,.F.);
#5879=ORIENTED_EDGE('',*,*,#4759,.T.);
#5880=ORIENTED_EDGE('',*,*,#4744,.T.);
#5881=ORIENTED_EDGE('',*,*,#4759,.F.);
#5882=ORIENTED_EDGE('',*,*,#4760,.F.);
#5883=ORIENTED_EDGE('',*,*,#4761,.T.);
#5884=ORIENTED_EDGE('',*,*,#4748,.T.);
#5885=ORIENTED_EDGE('',*,*,#4761,.F.);
#5886=ORIENTED_EDGE('',*,*,#4753,.F.);
#5887=ORIENTED_EDGE('',*,*,#4762,.T.);
#5888=ORIENTED_EDGE('',*,*,#4763,.F.);
#5889=ORIENTED_EDGE('',*,*,#4762,.F.);
#5890=ORIENTED_EDGE('',*,*,#4764,.F.);
#5891=ORIENTED_EDGE('',*,*,#4765,.T.);
#5892=ORIENTED_EDGE('',*,*,#4766,.T.);
#5893=ORIENTED_EDGE('',*,*,#4765,.F.);
#5894=ORIENTED_EDGE('',*,*,#4749,.F.);
#5895=ORIENTED_EDGE('',*,*,#4715,.F.);
#5896=ORIENTED_EDGE('',*,*,#4767,.T.);
#5897=ORIENTED_EDGE('',*,*,#4768,.T.);
#5898=ORIENTED_EDGE('',*,*,#4767,.F.);
#5899=ORIENTED_EDGE('',*,*,#4738,.T.);
#5900=ORIENTED_EDGE('',*,*,#4752,.F.);
#5901=ORIENTED_EDGE('',*,*,#4711,.F.);
#5902=ORIENTED_EDGE('',*,*,#4742,.T.);
#5903=ORIENTED_EDGE('',*,*,#4751,.F.);
#5904=ORIENTED_EDGE('',*,*,#4707,.F.);
#5905=ORIENTED_EDGE('',*,*,#4746,.T.);
#5906=ORIENTED_EDGE('',*,*,#4750,.F.);
#5907=ORIENTED_EDGE('',*,*,#4719,.F.);
#5908=ORIENTED_EDGE('',*,*,#4734,.T.);
#5909=ORIENTED_EDGE('',*,*,#4763,.T.);
#5910=ORIENTED_EDGE('',*,*,#4764,.T.);
#5911=ORIENTED_EDGE('',*,*,#4768,.F.);
#5912=ORIENTED_EDGE('',*,*,#4766,.F.);
#5913=ORIENTED_EDGE('',*,*,#4760,.T.);
#5914=ORIENTED_EDGE('',*,*,#4758,.T.);
#5915=ORIENTED_EDGE('',*,*,#4756,.T.);
#5916=ORIENTED_EDGE('',*,*,#4754,.T.);
#5917=ORIENTED_EDGE('',*,*,#4769,.F.);
#5918=ORIENTED_EDGE('',*,*,#4770,.T.);
#5919=ORIENTED_EDGE('',*,*,#4771,.F.);
#5920=ORIENTED_EDGE('',*,*,#4770,.F.);
#5921=ORIENTED_EDGE('',*,*,#4772,.F.);
#5922=ORIENTED_EDGE('',*,*,#4773,.T.);
#5923=ORIENTED_EDGE('',*,*,#4774,.F.);
#5924=ORIENTED_EDGE('',*,*,#4773,.F.);
#5925=ORIENTED_EDGE('',*,*,#4775,.F.);
#5926=ORIENTED_EDGE('',*,*,#4776,.T.);
#5927=ORIENTED_EDGE('',*,*,#4777,.F.);
#5928=ORIENTED_EDGE('',*,*,#4776,.F.);
#5929=ORIENTED_EDGE('',*,*,#4778,.F.);
#5930=ORIENTED_EDGE('',*,*,#4779,.T.);
#5931=ORIENTED_EDGE('',*,*,#4780,.F.);
#5932=ORIENTED_EDGE('',*,*,#4779,.F.);
#5933=ORIENTED_EDGE('',*,*,#4781,.F.);
#5934=ORIENTED_EDGE('',*,*,#4782,.T.);
#5935=ORIENTED_EDGE('',*,*,#4783,.T.);
#5936=ORIENTED_EDGE('',*,*,#4782,.F.);
#5937=ORIENTED_EDGE('',*,*,#4783,.F.);
#5938=ORIENTED_EDGE('',*,*,#4784,.F.);
#5939=ORIENTED_EDGE('',*,*,#4785,.F.);
#5940=ORIENTED_EDGE('',*,*,#4786,.T.);
#5941=ORIENTED_EDGE('',*,*,#4784,.T.);
#5942=ORIENTED_EDGE('',*,*,#4786,.F.);
#5943=ORIENTED_EDGE('',*,*,#4787,.F.);
#5944=ORIENTED_EDGE('',*,*,#4788,.T.);
#5945=ORIENTED_EDGE('',*,*,#4789,.T.);
#5946=ORIENTED_EDGE('',*,*,#4788,.F.);
#5947=ORIENTED_EDGE('',*,*,#4787,.T.);
#5948=ORIENTED_EDGE('',*,*,#4785,.T.);
#5949=ORIENTED_EDGE('',*,*,#4780,.T.);
#5950=ORIENTED_EDGE('',*,*,#4777,.T.);
#5951=ORIENTED_EDGE('',*,*,#4774,.T.);
#5952=ORIENTED_EDGE('',*,*,#4771,.T.);
#5953=ORIENTED_EDGE('',*,*,#4789,.F.);
#5954=ORIENTED_EDGE('',*,*,#4781,.T.);
#5955=ORIENTED_EDGE('',*,*,#4778,.T.);
#5956=ORIENTED_EDGE('',*,*,#4775,.T.);
#5957=ORIENTED_EDGE('',*,*,#4772,.T.);
#5958=ORIENTED_EDGE('',*,*,#4769,.T.);
#5959=ORIENTED_EDGE('',*,*,#4790,.T.);
#5960=ORIENTED_EDGE('',*,*,#4791,.T.);
#5961=ORIENTED_EDGE('',*,*,#4792,.T.);
#5962=ORIENTED_EDGE('',*,*,#4793,.F.);
#5963=ORIENTED_EDGE('',*,*,#4794,.T.);
#5964=ORIENTED_EDGE('',*,*,#4795,.T.);
#5965=ORIENTED_EDGE('',*,*,#4796,.T.);
#5966=ORIENTED_EDGE('',*,*,#4791,.F.);
#5967=ORIENTED_EDGE('',*,*,#4797,.T.);
#5968=ORIENTED_EDGE('',*,*,#4798,.T.);
#5969=ORIENTED_EDGE('',*,*,#4799,.T.);
#5970=ORIENTED_EDGE('',*,*,#4795,.F.);
#5971=ORIENTED_EDGE('',*,*,#4800,.T.);
#5972=ORIENTED_EDGE('',*,*,#4801,.T.);
#5973=ORIENTED_EDGE('',*,*,#4802,.T.);
#5974=ORIENTED_EDGE('',*,*,#4798,.F.);
#5975=ORIENTED_EDGE('',*,*,#4803,.T.);
#5976=ORIENTED_EDGE('',*,*,#4804,.T.);
#5977=ORIENTED_EDGE('',*,*,#4805,.T.);
#5978=ORIENTED_EDGE('',*,*,#4801,.F.);
#5979=ORIENTED_EDGE('',*,*,#4806,.T.);
#5980=ORIENTED_EDGE('',*,*,#4793,.T.);
#5981=ORIENTED_EDGE('',*,*,#4807,.T.);
#5982=ORIENTED_EDGE('',*,*,#4804,.F.);
#5983=ORIENTED_EDGE('',*,*,#4806,.F.);
#5984=ORIENTED_EDGE('',*,*,#4803,.F.);
#5985=ORIENTED_EDGE('',*,*,#4800,.F.);
#5986=ORIENTED_EDGE('',*,*,#4797,.F.);
#5987=ORIENTED_EDGE('',*,*,#4794,.F.);
#5988=ORIENTED_EDGE('',*,*,#4790,.F.);
#5989=ORIENTED_EDGE('',*,*,#4807,.F.);
#5990=ORIENTED_EDGE('',*,*,#4792,.F.);
#5991=ORIENTED_EDGE('',*,*,#4796,.F.);
#5992=ORIENTED_EDGE('',*,*,#4799,.F.);
#5993=ORIENTED_EDGE('',*,*,#4802,.F.);
#5994=ORIENTED_EDGE('',*,*,#4805,.F.);
#5995=ORIENTED_EDGE('',*,*,#4808,.F.);
#5996=ORIENTED_EDGE('',*,*,#4809,.F.);
#5997=ORIENTED_EDGE('',*,*,#4810,.F.);
#5998=ORIENTED_EDGE('',*,*,#4811,.T.);
#5999=ORIENTED_EDGE('',*,*,#4809,.T.);
#6000=ORIENTED_EDGE('',*,*,#4811,.F.);
#6001=ORIENTED_EDGE('',*,*,#4812,.F.);
#6002=ORIENTED_EDGE('',*,*,#4813,.T.);
#6003=ORIENTED_EDGE('',*,*,#4810,.T.);
#6004=ORIENTED_EDGE('',*,*,#4813,.F.);
#6005=ORIENTED_EDGE('',*,*,#4814,.F.);
#6006=ORIENTED_EDGE('',*,*,#4815,.T.);
#6007=ORIENTED_EDGE('',*,*,#4812,.T.);
#6008=ORIENTED_EDGE('',*,*,#4815,.F.);
#6009=ORIENTED_EDGE('',*,*,#4814,.T.);
#6010=ORIENTED_EDGE('',*,*,#4816,.F.);
#6011=ORIENTED_EDGE('',*,*,#4817,.F.);
#6012=ORIENTED_EDGE('',*,*,#4818,.T.);
#6013=ORIENTED_EDGE('',*,*,#4816,.T.);
#6014=ORIENTED_EDGE('',*,*,#4818,.F.);
#6015=ORIENTED_EDGE('',*,*,#4808,.T.);
#6016=ORIENTED_EDGE('',*,*,#4819,.T.);
#6017=ORIENTED_EDGE('',*,*,#4817,.T.);
#6018=ORIENTED_EDGE('',*,*,#4819,.F.);
#6019=ORIENTED_EDGE('',*,*,#4820,.F.);
#6020=ORIENTED_EDGE('',*,*,#4821,.F.);
#6021=ORIENTED_EDGE('',*,*,#4822,.T.);
#6022=ORIENTED_EDGE('',*,*,#4823,.F.);
#6023=ORIENTED_EDGE('',*,*,#4824,.F.);
#6024=ORIENTED_EDGE('',*,*,#4822,.F.);
#6025=ORIENTED_EDGE('',*,*,#4823,.T.);
#6026=ORIENTED_EDGE('',*,*,#4824,.T.);
#6027=ORIENTED_EDGE('',*,*,#4825,.T.);
#6028=ORIENTED_EDGE('',*,*,#4826,.T.);
#6029=ORIENTED_EDGE('',*,*,#4825,.F.);
#6030=ORIENTED_EDGE('',*,*,#4827,.T.);
#6031=ORIENTED_EDGE('',*,*,#4828,.T.);
#6032=ORIENTED_EDGE('',*,*,#4829,.F.);
#6033=ORIENTED_EDGE('',*,*,#4828,.F.);
#6034=ORIENTED_EDGE('',*,*,#4829,.T.);
#6035=ORIENTED_EDGE('',*,*,#4830,.T.);
#6036=ORIENTED_EDGE('',*,*,#4831,.F.);
#6037=ORIENTED_EDGE('',*,*,#4830,.F.);
#6038=ORIENTED_EDGE('',*,*,#4826,.F.);
#6039=ORIENTED_EDGE('',*,*,#4831,.T.);
#6040=ORIENTED_EDGE('',*,*,#4832,.F.);
#6041=ORIENTED_EDGE('',*,*,#4833,.T.);
#6042=ORIENTED_EDGE('',*,*,#4820,.T.);
#6043=ORIENTED_EDGE('',*,*,#4821,.T.);
#6044=ORIENTED_EDGE('',*,*,#4833,.F.);
#6045=ORIENTED_EDGE('',*,*,#4832,.T.);
#6046=ORIENTED_EDGE('',*,*,#4834,.F.);
#6047=ORIENTED_EDGE('',*,*,#4834,.T.);
#6048=ORIENTED_EDGE('',*,*,#4835,.T.);
#6049=ORIENTED_EDGE('',*,*,#4827,.F.);
#6050=ORIENTED_EDGE('',*,*,#4835,.F.);
#6051=ORIENTED_EDGE('',*,*,#4836,.F.);
#6052=ORIENTED_EDGE('',*,*,#4837,.F.);
#6053=ORIENTED_EDGE('',*,*,#4838,.T.);
#6054=ORIENTED_EDGE('',*,*,#4839,.F.);
#6055=ORIENTED_EDGE('',*,*,#4840,.F.);
#6056=ORIENTED_EDGE('',*,*,#4838,.F.);
#6057=ORIENTED_EDGE('',*,*,#4841,.T.);
#6058=ORIENTED_EDGE('',*,*,#4842,.T.);
#6059=ORIENTED_EDGE('',*,*,#4839,.T.);
#6060=ORIENTED_EDGE('',*,*,#4840,.T.);
#6061=ORIENTED_EDGE('',*,*,#4842,.F.);
#6062=ORIENTED_EDGE('',*,*,#4843,.F.);
#6063=ORIENTED_EDGE('',*,*,#4844,.T.);
#6064=ORIENTED_EDGE('',*,*,#4845,.F.);
#6065=ORIENTED_EDGE('',*,*,#4846,.T.);
#6066=ORIENTED_EDGE('',*,*,#4843,.T.);
#6067=ORIENTED_EDGE('',*,*,#4846,.F.);
#6068=ORIENTED_EDGE('',*,*,#4847,.F.);
#6069=ORIENTED_EDGE('',*,*,#4848,.T.);
#6070=ORIENTED_EDGE('',*,*,#4845,.T.);
#6071=ORIENTED_EDGE('',*,*,#4848,.F.);
#6072=ORIENTED_EDGE('',*,*,#4849,.F.);
#6073=ORIENTED_EDGE('',*,*,#4850,.T.);
#6074=ORIENTED_EDGE('',*,*,#4847,.T.);
#6075=ORIENTED_EDGE('',*,*,#4850,.F.);
#6076=ORIENTED_EDGE('',*,*,#4849,.T.);
#6077=ORIENTED_EDGE('',*,*,#4841,.F.);
#6078=ORIENTED_EDGE('',*,*,#4836,.T.);
#6079=ORIENTED_EDGE('',*,*,#4837,.T.);
#6080=ORIENTED_EDGE('',*,*,#4851,.T.);
#6081=ORIENTED_EDGE('',*,*,#4844,.F.);
#6082=ORIENTED_EDGE('',*,*,#4851,.F.);
#6083=ORIENTED_EDGE('',*,*,#4852,.T.);
#6084=ORIENTED_EDGE('',*,*,#4852,.F.);
#6085=ORIENTED_EDGE('',*,*,#4853,.T.);
#6086=ORIENTED_EDGE('',*,*,#4853,.F.);
#6087=ORIENTED_EDGE('',*,*,#4854,.T.);
#6088=ORIENTED_EDGE('',*,*,#4854,.F.);
#6089=ORIENTED_EDGE('',*,*,#4855,.T.);
#6090=ORIENTED_EDGE('',*,*,#4855,.F.);
#6091=ORIENTED_EDGE('',*,*,#4856,.T.);
#6092=ORIENTED_EDGE('',*,*,#4856,.F.);
#6093=ORIENTED_EDGE('',*,*,#4857,.T.);
#6094=ORIENTED_EDGE('',*,*,#4857,.F.);
#6095=ORIENTED_EDGE('',*,*,#4858,.T.);
#6096=ORIENTED_EDGE('',*,*,#4858,.F.);
#6097=ORIENTED_EDGE('',*,*,#4859,.T.);
#6098=ORIENTED_EDGE('',*,*,#4859,.F.);
#6099=ORIENTED_EDGE('',*,*,#4860,.T.);
#6100=ORIENTED_EDGE('',*,*,#4860,.F.);
#6101=ORIENTED_EDGE('',*,*,#4861,.F.);
#6102=ORIENTED_EDGE('',*,*,#4862,.F.);
#6103=ORIENTED_EDGE('',*,*,#4863,.F.);
#6104=ORIENTED_EDGE('',*,*,#4864,.F.);
#6105=ORIENTED_EDGE('',*,*,#4863,.T.);
#6106=ORIENTED_EDGE('',*,*,#4865,.F.);
#6107=ORIENTED_EDGE('',*,*,#4866,.T.);
#6108=ORIENTED_EDGE('',*,*,#4867,.F.);
#6109=ORIENTED_EDGE('',*,*,#4868,.T.);
#6110=ORIENTED_EDGE('',*,*,#4869,.F.);
#6111=ORIENTED_EDGE('',*,*,#4870,.T.);
#6112=ORIENTED_EDGE('',*,*,#4871,.F.);
#6113=ORIENTED_EDGE('',*,*,#4872,.T.);
#6114=ORIENTED_EDGE('',*,*,#4873,.F.);
#6115=ORIENTED_EDGE('',*,*,#4872,.F.);
#6116=ORIENTED_EDGE('',*,*,#4874,.F.);
#6117=ORIENTED_EDGE('',*,*,#4875,.T.);
#6118=ORIENTED_EDGE('',*,*,#4876,.F.);
#6119=ORIENTED_EDGE('',*,*,#4877,.T.);
#6120=ORIENTED_EDGE('',*,*,#4878,.F.);
#6121=ORIENTED_EDGE('',*,*,#4879,.T.);
#6122=ORIENTED_EDGE('',*,*,#4880,.F.);
#6123=ORIENTED_EDGE('',*,*,#4881,.T.);
#6124=ORIENTED_EDGE('',*,*,#4882,.F.);
#6125=ORIENTED_EDGE('',*,*,#4883,.T.);
#6126=ORIENTED_EDGE('',*,*,#4884,.F.);
#6127=ORIENTED_EDGE('',*,*,#4862,.T.);
#6128=ORIENTED_EDGE('',*,*,#4885,.T.);
#6129=ORIENTED_EDGE('',*,*,#4886,.T.);
#6130=ORIENTED_EDGE('',*,*,#4865,.T.);
#6131=ORIENTED_EDGE('',*,*,#4887,.F.);
#6132=ORIENTED_EDGE('',*,*,#4888,.F.);
#6133=ORIENTED_EDGE('',*,*,#4866,.F.);
#6134=ORIENTED_EDGE('',*,*,#4886,.F.);
#6135=ORIENTED_EDGE('',*,*,#4888,.T.);
#6136=ORIENTED_EDGE('',*,*,#4889,.T.);
#6137=ORIENTED_EDGE('',*,*,#4890,.T.);
#6138=ORIENTED_EDGE('',*,*,#4867,.T.);
#6139=ORIENTED_EDGE('',*,*,#4891,.F.);
#6140=ORIENTED_EDGE('',*,*,#4892,.F.);
#6141=ORIENTED_EDGE('',*,*,#4868,.F.);
#6142=ORIENTED_EDGE('',*,*,#4890,.F.);
#6143=ORIENTED_EDGE('',*,*,#4892,.T.);
#6144=ORIENTED_EDGE('',*,*,#4893,.T.);
#6145=ORIENTED_EDGE('',*,*,#4894,.T.);
#6146=ORIENTED_EDGE('',*,*,#4869,.T.);
#6147=ORIENTED_EDGE('',*,*,#4895,.F.);
#6148=ORIENTED_EDGE('',*,*,#4896,.F.);
#6149=ORIENTED_EDGE('',*,*,#4870,.F.);
#6150=ORIENTED_EDGE('',*,*,#4894,.F.);
#6151=ORIENTED_EDGE('',*,*,#4896,.T.);
#6152=ORIENTED_EDGE('',*,*,#4897,.T.);
#6153=ORIENTED_EDGE('',*,*,#4898,.T.);
#6154=ORIENTED_EDGE('',*,*,#4899,.T.);
#6155=ORIENTED_EDGE('',*,*,#4874,.T.);
#6156=ORIENTED_EDGE('',*,*,#4871,.T.);
#6157=ORIENTED_EDGE('',*,*,#4900,.F.);
#6158=ORIENTED_EDGE('',*,*,#4901,.F.);
#6159=ORIENTED_EDGE('',*,*,#4875,.F.);
#6160=ORIENTED_EDGE('',*,*,#4899,.F.);
#6161=ORIENTED_EDGE('',*,*,#4901,.T.);
#6162=ORIENTED_EDGE('',*,*,#4902,.T.);
#6163=ORIENTED_EDGE('',*,*,#4903,.T.);
#6164=ORIENTED_EDGE('',*,*,#4876,.T.);
#6165=ORIENTED_EDGE('',*,*,#4904,.F.);
#6166=ORIENTED_EDGE('',*,*,#4905,.F.);
#6167=ORIENTED_EDGE('',*,*,#4877,.F.);
#6168=ORIENTED_EDGE('',*,*,#4903,.F.);
#6169=ORIENTED_EDGE('',*,*,#4905,.T.);
#6170=ORIENTED_EDGE('',*,*,#4906,.T.);
#6171=ORIENTED_EDGE('',*,*,#4907,.T.);
#6172=ORIENTED_EDGE('',*,*,#4878,.T.);
#6173=ORIENTED_EDGE('',*,*,#4908,.F.);
#6174=ORIENTED_EDGE('',*,*,#4909,.F.);
#6175=ORIENTED_EDGE('',*,*,#4879,.F.);
#6176=ORIENTED_EDGE('',*,*,#4907,.F.);
#6177=ORIENTED_EDGE('',*,*,#4909,.T.);
#6178=ORIENTED_EDGE('',*,*,#4910,.T.);
#6179=ORIENTED_EDGE('',*,*,#4911,.T.);
#6180=ORIENTED_EDGE('',*,*,#4880,.T.);
#6181=ORIENTED_EDGE('',*,*,#4881,.F.);
#6182=ORIENTED_EDGE('',*,*,#4911,.F.);
#6183=ORIENTED_EDGE('',*,*,#4912,.F.);
#6184=ORIENTED_EDGE('',*,*,#4913,.F.);
#6185=ORIENTED_EDGE('',*,*,#4914,.F.);
#6186=ORIENTED_EDGE('',*,*,#4915,.T.);
#6187=ORIENTED_EDGE('',*,*,#4897,.F.);
#6188=ORIENTED_EDGE('',*,*,#4895,.T.);
#6189=ORIENTED_EDGE('',*,*,#4893,.F.);
#6190=ORIENTED_EDGE('',*,*,#4891,.T.);
#6191=ORIENTED_EDGE('',*,*,#4889,.F.);
#6192=ORIENTED_EDGE('',*,*,#4887,.T.);
#6193=ORIENTED_EDGE('',*,*,#4885,.F.);
#6194=ORIENTED_EDGE('',*,*,#4861,.T.);
#6195=ORIENTED_EDGE('',*,*,#4916,.F.);
#6196=ORIENTED_EDGE('',*,*,#4917,.T.);
#6197=ORIENTED_EDGE('',*,*,#4918,.F.);
#6198=ORIENTED_EDGE('',*,*,#4912,.T.);
#6199=ORIENTED_EDGE('',*,*,#4910,.F.);
#6200=ORIENTED_EDGE('',*,*,#4908,.T.);
#6201=ORIENTED_EDGE('',*,*,#4906,.F.);
#6202=ORIENTED_EDGE('',*,*,#4904,.T.);
#6203=ORIENTED_EDGE('',*,*,#4902,.F.);
#6204=ORIENTED_EDGE('',*,*,#4900,.T.);
#6205=ORIENTED_EDGE('',*,*,#4898,.F.);
#6206=ORIENTED_EDGE('',*,*,#4915,.F.);
#6207=ORIENTED_EDGE('',*,*,#4864,.T.);
#6208=ORIENTED_EDGE('',*,*,#4884,.T.);
#6209=ORIENTED_EDGE('',*,*,#4919,.T.);
#6210=ORIENTED_EDGE('',*,*,#4916,.T.);
#6211=ORIENTED_EDGE('',*,*,#4883,.F.);
#6212=ORIENTED_EDGE('',*,*,#4920,.F.);
#6213=ORIENTED_EDGE('',*,*,#4917,.F.);
#6214=ORIENTED_EDGE('',*,*,#4919,.F.);
#6215=ORIENTED_EDGE('',*,*,#4873,.T.);
#6216=ORIENTED_EDGE('',*,*,#4914,.T.);
#6217=ORIENTED_EDGE('',*,*,#4913,.T.);
#6218=ORIENTED_EDGE('',*,*,#4918,.T.);
#6219=ORIENTED_EDGE('',*,*,#4920,.T.);
#6220=ORIENTED_EDGE('',*,*,#4882,.T.);
#6221=ORIENTED_EDGE('',*,*,#4921,.F.);
#6222=ORIENTED_EDGE('',*,*,#4922,.T.);
#6223=ORIENTED_EDGE('',*,*,#4923,.F.);
#6224=ORIENTED_EDGE('',*,*,#4924,.T.);
#6225=ORIENTED_EDGE('',*,*,#4921,.T.);
#6226=ORIENTED_EDGE('',*,*,#4924,.F.);
#6227=ORIENTED_EDGE('',*,*,#4923,.T.);
#6228=ORIENTED_EDGE('',*,*,#4925,.F.);
#6229=ORIENTED_EDGE('',*,*,#4925,.T.);
#6230=ORIENTED_EDGE('',*,*,#4926,.T.);
#6231=ORIENTED_EDGE('',*,*,#4922,.F.);
#6232=ORIENTED_EDGE('',*,*,#4926,.F.);
#6233=ORIENTED_EDGE('',*,*,#4927,.F.);
#6234=ORIENTED_EDGE('',*,*,#4928,.T.);
#6235=ORIENTED_EDGE('',*,*,#4929,.F.);
#6236=ORIENTED_EDGE('',*,*,#4930,.T.);
#6237=ORIENTED_EDGE('',*,*,#4927,.T.);
#6238=ORIENTED_EDGE('',*,*,#4930,.F.);
#6239=ORIENTED_EDGE('',*,*,#4929,.T.);
#6240=ORIENTED_EDGE('',*,*,#4931,.F.);
#6241=ORIENTED_EDGE('',*,*,#4931,.T.);
#6242=ORIENTED_EDGE('',*,*,#4932,.T.);
#6243=ORIENTED_EDGE('',*,*,#4928,.F.);
#6244=ORIENTED_EDGE('',*,*,#4932,.F.);
#6245=ORIENTED_EDGE('',*,*,#4933,.T.);
#6246=ORIENTED_EDGE('',*,*,#4934,.T.);
#6247=ORIENTED_EDGE('',*,*,#4935,.F.);
#6248=ORIENTED_EDGE('',*,*,#4936,.F.);
#6249=ORIENTED_EDGE('',*,*,#4937,.T.);
#6250=ORIENTED_EDGE('',*,*,#4936,.T.);
#6251=ORIENTED_EDGE('',*,*,#4938,.F.);
#6252=ORIENTED_EDGE('',*,*,#4939,.F.);
#6253=ORIENTED_EDGE('',*,*,#4940,.T.);
#6254=ORIENTED_EDGE('',*,*,#4939,.T.);
#6255=ORIENTED_EDGE('',*,*,#4941,.F.);
#6256=ORIENTED_EDGE('',*,*,#4942,.F.);
#6257=ORIENTED_EDGE('',*,*,#4943,.T.);
#6258=ORIENTED_EDGE('',*,*,#4942,.T.);
#6259=ORIENTED_EDGE('',*,*,#4944,.F.);
#6260=ORIENTED_EDGE('',*,*,#4934,.F.);
#6261=ORIENTED_EDGE('',*,*,#4944,.T.);
#6262=ORIENTED_EDGE('',*,*,#4941,.T.);
#6263=ORIENTED_EDGE('',*,*,#4938,.T.);
#6264=ORIENTED_EDGE('',*,*,#4935,.T.);
#6265=ORIENTED_EDGE('',*,*,#4943,.F.);
#6266=ORIENTED_EDGE('',*,*,#4933,.F.);
#6267=ORIENTED_EDGE('',*,*,#4937,.F.);
#6268=ORIENTED_EDGE('',*,*,#4940,.F.);
#6269=ORIENTED_EDGE('',*,*,#4945,.T.);
#6270=ORIENTED_EDGE('',*,*,#4946,.T.);
#6271=ORIENTED_EDGE('',*,*,#4947,.F.);
#6272=ORIENTED_EDGE('',*,*,#4948,.F.);
#6273=ORIENTED_EDGE('',*,*,#4949,.T.);
#6274=ORIENTED_EDGE('',*,*,#4948,.T.);
#6275=ORIENTED_EDGE('',*,*,#4950,.F.);
#6276=ORIENTED_EDGE('',*,*,#4951,.F.);
#6277=ORIENTED_EDGE('',*,*,#4952,.T.);
#6278=ORIENTED_EDGE('',*,*,#4951,.T.);
#6279=ORIENTED_EDGE('',*,*,#4953,.F.);
#6280=ORIENTED_EDGE('',*,*,#4954,.F.);
#6281=ORIENTED_EDGE('',*,*,#4955,.T.);
#6282=ORIENTED_EDGE('',*,*,#4954,.T.);
#6283=ORIENTED_EDGE('',*,*,#4956,.F.);
#6284=ORIENTED_EDGE('',*,*,#4946,.F.);
#6285=ORIENTED_EDGE('',*,*,#4956,.T.);
#6286=ORIENTED_EDGE('',*,*,#4953,.T.);
#6287=ORIENTED_EDGE('',*,*,#4950,.T.);
#6288=ORIENTED_EDGE('',*,*,#4947,.T.);
#6289=ORIENTED_EDGE('',*,*,#4955,.F.);
#6290=ORIENTED_EDGE('',*,*,#4945,.F.);
#6291=ORIENTED_EDGE('',*,*,#4949,.F.);
#6292=ORIENTED_EDGE('',*,*,#4952,.F.);
#6293=ORIENTED_EDGE('',*,*,#4957,.F.);
#6294=ORIENTED_EDGE('',*,*,#4958,.T.);
#6295=ORIENTED_EDGE('',*,*,#4959,.F.);
#6296=ORIENTED_EDGE('',*,*,#4958,.F.);
#6297=ORIENTED_EDGE('',*,*,#4957,.T.);
#6298=ORIENTED_EDGE('',*,*,#4960,.F.);
#6299=ORIENTED_EDGE('',*,*,#4961,.T.);
#6300=ORIENTED_EDGE('',*,*,#4962,.F.);
#6301=ORIENTED_EDGE('',*,*,#4961,.F.);
#6302=ORIENTED_EDGE('',*,*,#4960,.T.);
#6303=ORIENTED_EDGE('',*,*,#4963,.F.);
#6304=ORIENTED_EDGE('',*,*,#4964,.T.);
#6305=ORIENTED_EDGE('',*,*,#4965,.F.);
#6306=ORIENTED_EDGE('',*,*,#4964,.F.);
#6307=ORIENTED_EDGE('',*,*,#4963,.T.);
#6308=ORIENTED_EDGE('',*,*,#4966,.F.);
#6309=ORIENTED_EDGE('',*,*,#4967,.F.);
#6310=ORIENTED_EDGE('',*,*,#4968,.F.);
#6311=ORIENTED_EDGE('',*,*,#4969,.T.);
#6312=ORIENTED_EDGE('',*,*,#4966,.T.);
#6313=ORIENTED_EDGE('',*,*,#4969,.F.);
#6314=ORIENTED_EDGE('',*,*,#4967,.T.);
#6315=ORIENTED_EDGE('',*,*,#4970,.T.);
#6316=ORIENTED_EDGE('',*,*,#4971,.T.);
#6317=ORIENTED_EDGE('',*,*,#4970,.F.);
#6318=ORIENTED_EDGE('',*,*,#4968,.T.);
#6319=ORIENTED_EDGE('',*,*,#4959,.T.);
#6320=ORIENTED_EDGE('',*,*,#4962,.T.);
#6321=ORIENTED_EDGE('',*,*,#4965,.T.);
#6322=ORIENTED_EDGE('',*,*,#4971,.F.);
#6323=ORIENTED_EDGE('',*,*,#4972,.F.);
#6324=ORIENTED_EDGE('',*,*,#4973,.T.);
#6325=ORIENTED_EDGE('',*,*,#4974,.F.);
#6326=ORIENTED_EDGE('',*,*,#4973,.F.);
#6327=ORIENTED_EDGE('',*,*,#4975,.F.);
#6328=ORIENTED_EDGE('',*,*,#4976,.T.);
#6329=ORIENTED_EDGE('',*,*,#4977,.F.);
#6330=ORIENTED_EDGE('',*,*,#4976,.F.);
#6331=ORIENTED_EDGE('',*,*,#4978,.F.);
#6332=ORIENTED_EDGE('',*,*,#4979,.T.);
#6333=ORIENTED_EDGE('',*,*,#4980,.F.);
#6334=ORIENTED_EDGE('',*,*,#4979,.F.);
#6335=ORIENTED_EDGE('',*,*,#4981,.F.);
#6336=ORIENTED_EDGE('',*,*,#4982,.T.);
#6337=ORIENTED_EDGE('',*,*,#4983,.F.);
#6338=ORIENTED_EDGE('',*,*,#4982,.F.);
#6339=ORIENTED_EDGE('',*,*,#4984,.F.);
#6340=ORIENTED_EDGE('',*,*,#4985,.T.);
#6341=ORIENTED_EDGE('',*,*,#4986,.F.);
#6342=ORIENTED_EDGE('',*,*,#4985,.F.);
#6343=ORIENTED_EDGE('',*,*,#4987,.F.);
#6344=ORIENTED_EDGE('',*,*,#4988,.T.);
#6345=ORIENTED_EDGE('',*,*,#4989,.F.);
#6346=ORIENTED_EDGE('',*,*,#4988,.F.);
#6347=ORIENTED_EDGE('',*,*,#4990,.F.);
#6348=ORIENTED_EDGE('',*,*,#4991,.T.);
#6349=ORIENTED_EDGE('',*,*,#4992,.F.);
#6350=ORIENTED_EDGE('',*,*,#4991,.F.);
#6351=ORIENTED_EDGE('',*,*,#4993,.F.);
#6352=ORIENTED_EDGE('',*,*,#4994,.T.);
#6353=ORIENTED_EDGE('',*,*,#4995,.F.);
#6354=ORIENTED_EDGE('',*,*,#4994,.F.);
#6355=ORIENTED_EDGE('',*,*,#4996,.F.);
#6356=ORIENTED_EDGE('',*,*,#4997,.T.);
#6357=ORIENTED_EDGE('',*,*,#4998,.F.);
#6358=ORIENTED_EDGE('',*,*,#4997,.F.);
#6359=ORIENTED_EDGE('',*,*,#4999,.F.);
#6360=ORIENTED_EDGE('',*,*,#5000,.T.);
#6361=ORIENTED_EDGE('',*,*,#5001,.F.);
#6362=ORIENTED_EDGE('',*,*,#5000,.F.);
#6363=ORIENTED_EDGE('',*,*,#5002,.F.);
#6364=ORIENTED_EDGE('',*,*,#5003,.T.);
#6365=ORIENTED_EDGE('',*,*,#5004,.F.);
#6366=ORIENTED_EDGE('',*,*,#5003,.F.);
#6367=ORIENTED_EDGE('',*,*,#5005,.F.);
#6368=ORIENTED_EDGE('',*,*,#5006,.T.);
#6369=ORIENTED_EDGE('',*,*,#5007,.F.);
#6370=ORIENTED_EDGE('',*,*,#5006,.F.);
#6371=ORIENTED_EDGE('',*,*,#5008,.F.);
#6372=ORIENTED_EDGE('',*,*,#5009,.T.);
#6373=ORIENTED_EDGE('',*,*,#5010,.T.);
#6374=ORIENTED_EDGE('',*,*,#5009,.F.);
#6375=ORIENTED_EDGE('',*,*,#5008,.T.);
#6376=ORIENTED_EDGE('',*,*,#4983,.T.);
#6377=ORIENTED_EDGE('',*,*,#4986,.T.);
#6378=ORIENTED_EDGE('',*,*,#4989,.T.);
#6379=ORIENTED_EDGE('',*,*,#4992,.T.);
#6380=ORIENTED_EDGE('',*,*,#4995,.T.);
#6381=ORIENTED_EDGE('',*,*,#4998,.T.);
#6382=ORIENTED_EDGE('',*,*,#5001,.T.);
#6383=ORIENTED_EDGE('',*,*,#5004,.T.);
#6384=ORIENTED_EDGE('',*,*,#5007,.T.);
#6385=ORIENTED_EDGE('',*,*,#4980,.T.);
#6386=ORIENTED_EDGE('',*,*,#4977,.T.);
#6387=ORIENTED_EDGE('',*,*,#4974,.T.);
#6388=ORIENTED_EDGE('',*,*,#5010,.F.);
#6389=ORIENTED_EDGE('',*,*,#4981,.T.);
#6390=ORIENTED_EDGE('',*,*,#4984,.T.);
#6391=ORIENTED_EDGE('',*,*,#4987,.T.);
#6392=ORIENTED_EDGE('',*,*,#4990,.T.);
#6393=ORIENTED_EDGE('',*,*,#4993,.T.);
#6394=ORIENTED_EDGE('',*,*,#4996,.T.);
#6395=ORIENTED_EDGE('',*,*,#4999,.T.);
#6396=ORIENTED_EDGE('',*,*,#5002,.T.);
#6397=ORIENTED_EDGE('',*,*,#5005,.T.);
#6398=ORIENTED_EDGE('',*,*,#4978,.T.);
#6399=ORIENTED_EDGE('',*,*,#4975,.T.);
#6400=ORIENTED_EDGE('',*,*,#4972,.T.);
#6401=ORIENTED_EDGE('',*,*,#5011,.F.);
#6402=ORIENTED_EDGE('',*,*,#5012,.T.);
#6403=ORIENTED_EDGE('',*,*,#5013,.T.);
#6404=ORIENTED_EDGE('',*,*,#5014,.F.);
#6405=ORIENTED_EDGE('',*,*,#5015,.F.);
#6406=ORIENTED_EDGE('',*,*,#5016,.F.);
#6407=ORIENTED_EDGE('',*,*,#5013,.F.);
#6408=ORIENTED_EDGE('',*,*,#5017,.T.);
#6409=ORIENTED_EDGE('',*,*,#5018,.F.);
#6410=ORIENTED_EDGE('',*,*,#5017,.F.);
#6411=ORIENTED_EDGE('',*,*,#5012,.F.);
#6412=ORIENTED_EDGE('',*,*,#5019,.F.);
#6413=ORIENTED_EDGE('',*,*,#5015,.T.);
#6414=ORIENTED_EDGE('',*,*,#5020,.F.);
#6415=ORIENTED_EDGE('',*,*,#5021,.T.);
#6416=ORIENTED_EDGE('',*,*,#5022,.T.);
#6417=ORIENTED_EDGE('',*,*,#5021,.F.);
#6418=ORIENTED_EDGE('',*,*,#5016,.T.);
#6419=ORIENTED_EDGE('',*,*,#5019,.T.);
#6420=ORIENTED_EDGE('',*,*,#5014,.T.);
#6421=ORIENTED_EDGE('',*,*,#5011,.T.);
#6422=ORIENTED_EDGE('',*,*,#5023,.F.);
#6423=ORIENTED_EDGE('',*,*,#5024,.T.);
#6424=ORIENTED_EDGE('',*,*,#5025,.T.);
#6425=ORIENTED_EDGE('',*,*,#5024,.F.);
#6426=ORIENTED_EDGE('',*,*,#5018,.T.);
#6427=ORIENTED_EDGE('',*,*,#5023,.T.);
#6428=ORIENTED_EDGE('',*,*,#5020,.T.);
#6429=ORIENTED_EDGE('',*,*,#5025,.F.);
#6430=ORIENTED_EDGE('',*,*,#5022,.F.);
#6431=ORIENTED_EDGE('',*,*,#5026,.F.);
#6432=ORIENTED_EDGE('',*,*,#5027,.F.);
#6433=ORIENTED_EDGE('',*,*,#5028,.T.);
#6434=ORIENTED_EDGE('',*,*,#5026,.T.);
#6435=ORIENTED_EDGE('',*,*,#5028,.F.);
#6436=ORIENTED_EDGE('',*,*,#5029,.F.);
#6437=ORIENTED_EDGE('',*,*,#5030,.T.);
#6438=ORIENTED_EDGE('',*,*,#5027,.T.);
#6439=ORIENTED_EDGE('',*,*,#5030,.F.);
#6440=ORIENTED_EDGE('',*,*,#5031,.F.);
#6441=ORIENTED_EDGE('',*,*,#5032,.T.);
#6442=ORIENTED_EDGE('',*,*,#5029,.T.);
#6443=ORIENTED_EDGE('',*,*,#5032,.F.);
#6444=ORIENTED_EDGE('',*,*,#5031,.T.);
#6445=ORIENTED_EDGE('',*,*,#5033,.F.);
#6446=ORIENTED_EDGE('',*,*,#5034,.F.);
#6447=ORIENTED_EDGE('',*,*,#5035,.T.);
#6448=ORIENTED_EDGE('',*,*,#5033,.T.);
#6449=ORIENTED_EDGE('',*,*,#5035,.F.);
#6450=ORIENTED_EDGE('',*,*,#5036,.F.);
#6451=ORIENTED_EDGE('',*,*,#5037,.T.);
#6452=ORIENTED_EDGE('',*,*,#5034,.T.);
#6453=ORIENTED_EDGE('',*,*,#5037,.F.);
#6454=ORIENTED_EDGE('',*,*,#5038,.F.);
#6455=ORIENTED_EDGE('',*,*,#5039,.T.);
#6456=ORIENTED_EDGE('',*,*,#5036,.T.);
#6457=ORIENTED_EDGE('',*,*,#5039,.F.);
#6458=ORIENTED_EDGE('',*,*,#5038,.T.);
#6459=ORIENTED_EDGE('',*,*,#5040,.T.);
#6460=ORIENTED_EDGE('',*,*,#5041,.T.);
#6461=ORIENTED_EDGE('',*,*,#5042,.T.);
#6462=ORIENTED_EDGE('',*,*,#5043,.F.);
#6463=ORIENTED_EDGE('',*,*,#5044,.T.);
#6464=ORIENTED_EDGE('',*,*,#5045,.T.);
#6465=ORIENTED_EDGE('',*,*,#5046,.T.);
#6466=ORIENTED_EDGE('',*,*,#5041,.F.);
#6467=ORIENTED_EDGE('',*,*,#5047,.T.);
#6468=ORIENTED_EDGE('',*,*,#5048,.T.);
#6469=ORIENTED_EDGE('',*,*,#5049,.T.);
#6470=ORIENTED_EDGE('',*,*,#5045,.F.);
#6471=ORIENTED_EDGE('',*,*,#5050,.T.);
#6472=ORIENTED_EDGE('',*,*,#5051,.T.);
#6473=ORIENTED_EDGE('',*,*,#5052,.T.);
#6474=ORIENTED_EDGE('',*,*,#5048,.F.);
#6475=ORIENTED_EDGE('',*,*,#5053,.T.);
#6476=ORIENTED_EDGE('',*,*,#5054,.T.);
#6477=ORIENTED_EDGE('',*,*,#5055,.T.);
#6478=ORIENTED_EDGE('',*,*,#5051,.F.);
#6479=ORIENTED_EDGE('',*,*,#5056,.T.);
#6480=ORIENTED_EDGE('',*,*,#5043,.T.);
#6481=ORIENTED_EDGE('',*,*,#5057,.T.);
#6482=ORIENTED_EDGE('',*,*,#5054,.F.);
#6483=ORIENTED_EDGE('',*,*,#5056,.F.);
#6484=ORIENTED_EDGE('',*,*,#5053,.F.);
#6485=ORIENTED_EDGE('',*,*,#5050,.F.);
#6486=ORIENTED_EDGE('',*,*,#5047,.F.);
#6487=ORIENTED_EDGE('',*,*,#5044,.F.);
#6488=ORIENTED_EDGE('',*,*,#5040,.F.);
#6489=ORIENTED_EDGE('',*,*,#5057,.F.);
#6490=ORIENTED_EDGE('',*,*,#5042,.F.);
#6491=ORIENTED_EDGE('',*,*,#5046,.F.);
#6492=ORIENTED_EDGE('',*,*,#5049,.F.);
#6493=ORIENTED_EDGE('',*,*,#5052,.F.);
#6494=ORIENTED_EDGE('',*,*,#5055,.F.);
#6495=ORIENTED_EDGE('',*,*,#5058,.F.);
#6496=ORIENTED_EDGE('',*,*,#5059,.T.);
#6497=ORIENTED_EDGE('',*,*,#5060,.T.);
#6498=ORIENTED_EDGE('',*,*,#5061,.F.);
#6499=ORIENTED_EDGE('',*,*,#5062,.F.);
#6500=ORIENTED_EDGE('',*,*,#5063,.T.);
#6501=ORIENTED_EDGE('',*,*,#5064,.T.);
#6502=ORIENTED_EDGE('',*,*,#5059,.F.);
#6503=ORIENTED_EDGE('',*,*,#5065,.F.);
#6504=ORIENTED_EDGE('',*,*,#5066,.T.);
#6505=ORIENTED_EDGE('',*,*,#5067,.T.);
#6506=ORIENTED_EDGE('',*,*,#5063,.F.);
#6507=ORIENTED_EDGE('',*,*,#5068,.F.);
#6508=ORIENTED_EDGE('',*,*,#5069,.T.);
#6509=ORIENTED_EDGE('',*,*,#5070,.T.);
#6510=ORIENTED_EDGE('',*,*,#5066,.F.);
#6511=ORIENTED_EDGE('',*,*,#5071,.F.);
#6512=ORIENTED_EDGE('',*,*,#5072,.T.);
#6513=ORIENTED_EDGE('',*,*,#5073,.T.);
#6514=ORIENTED_EDGE('',*,*,#5069,.F.);
#6515=ORIENTED_EDGE('',*,*,#5074,.F.);
#6516=ORIENTED_EDGE('',*,*,#5061,.T.);
#6517=ORIENTED_EDGE('',*,*,#5075,.T.);
#6518=ORIENTED_EDGE('',*,*,#5072,.F.);
#6519=ORIENTED_EDGE('',*,*,#5075,.F.);
#6520=ORIENTED_EDGE('',*,*,#5060,.F.);
#6521=ORIENTED_EDGE('',*,*,#5064,.F.);
#6522=ORIENTED_EDGE('',*,*,#5067,.F.);
#6523=ORIENTED_EDGE('',*,*,#5070,.F.);
#6524=ORIENTED_EDGE('',*,*,#5073,.F.);
#6525=ORIENTED_EDGE('',*,*,#5076,.F.);
#6526=ORIENTED_EDGE('',*,*,#5058,.T.);
#6527=ORIENTED_EDGE('',*,*,#5074,.T.);
#6528=ORIENTED_EDGE('',*,*,#5071,.T.);
#6529=ORIENTED_EDGE('',*,*,#5068,.T.);
#6530=ORIENTED_EDGE('',*,*,#5065,.T.);
#6531=ORIENTED_EDGE('',*,*,#5062,.T.);
#6532=ORIENTED_EDGE('',*,*,#5077,.F.);
#6533=ORIENTED_EDGE('',*,*,#5078,.T.);
#6534=ORIENTED_EDGE('',*,*,#5076,.T.);
#6535=ORIENTED_EDGE('',*,*,#5078,.F.);
#6536=ORIENTED_EDGE('',*,*,#5079,.F.);
#6537=ORIENTED_EDGE('',*,*,#5080,.T.);
#6538=ORIENTED_EDGE('',*,*,#5077,.T.);
#6539=ORIENTED_EDGE('',*,*,#5080,.F.);
#6540=ORIENTED_EDGE('',*,*,#5081,.F.);
#6541=ORIENTED_EDGE('',*,*,#5082,.T.);
#6542=ORIENTED_EDGE('',*,*,#5079,.T.);
#6543=ORIENTED_EDGE('',*,*,#5082,.F.);
#6544=ORIENTED_EDGE('',*,*,#5081,.T.);
#6545=ORIENTED_EDGE('',*,*,#5083,.F.);
#6546=ORIENTED_EDGE('',*,*,#5084,.T.);
#6547=ORIENTED_EDGE('',*,*,#5085,.F.);
#6548=ORIENTED_EDGE('',*,*,#5084,.F.);
#6549=ORIENTED_EDGE('',*,*,#5086,.F.);
#6550=ORIENTED_EDGE('',*,*,#5087,.T.);
#6551=ORIENTED_EDGE('',*,*,#5088,.F.);
#6552=ORIENTED_EDGE('',*,*,#5087,.F.);
#6553=ORIENTED_EDGE('',*,*,#5089,.F.);
#6554=ORIENTED_EDGE('',*,*,#5090,.T.);
#6555=ORIENTED_EDGE('',*,*,#5091,.F.);
#6556=ORIENTED_EDGE('',*,*,#5090,.F.);
#6557=ORIENTED_EDGE('',*,*,#5092,.F.);
#6558=ORIENTED_EDGE('',*,*,#5093,.T.);
#6559=ORIENTED_EDGE('',*,*,#5094,.F.);
#6560=ORIENTED_EDGE('',*,*,#5093,.F.);
#6561=ORIENTED_EDGE('',*,*,#5095,.F.);
#6562=ORIENTED_EDGE('',*,*,#5096,.T.);
#6563=ORIENTED_EDGE('',*,*,#5097,.F.);
#6564=ORIENTED_EDGE('',*,*,#5096,.F.);
#6565=ORIENTED_EDGE('',*,*,#5098,.F.);
#6566=ORIENTED_EDGE('',*,*,#5099,.T.);
#6567=ORIENTED_EDGE('',*,*,#5100,.F.);
#6568=ORIENTED_EDGE('',*,*,#5099,.F.);
#6569=ORIENTED_EDGE('',*,*,#5101,.F.);
#6570=ORIENTED_EDGE('',*,*,#5102,.T.);
#6571=ORIENTED_EDGE('',*,*,#5103,.F.);
#6572=ORIENTED_EDGE('',*,*,#5104,.F.);
#6573=ORIENTED_EDGE('',*,*,#5105,.F.);
#6574=ORIENTED_EDGE('',*,*,#5106,.F.);
#6575=ORIENTED_EDGE('',*,*,#5107,.F.);
#6576=ORIENTED_EDGE('',*,*,#5108,.F.);
#6577=ORIENTED_EDGE('',*,*,#5109,.F.);
#6578=ORIENTED_EDGE('',*,*,#5108,.T.);
#6579=ORIENTED_EDGE('',*,*,#5110,.F.);
#6580=ORIENTED_EDGE('',*,*,#5102,.F.);
#6581=ORIENTED_EDGE('',*,*,#5110,.T.);
#6582=ORIENTED_EDGE('',*,*,#5107,.T.);
#6583=ORIENTED_EDGE('',*,*,#5111,.F.);
#6584=ORIENTED_EDGE('',*,*,#5103,.T.);
#6585=ORIENTED_EDGE('',*,*,#5100,.T.);
#6586=ORIENTED_EDGE('',*,*,#5109,.T.);
#6587=ORIENTED_EDGE('',*,*,#5101,.T.);
#6588=ORIENTED_EDGE('',*,*,#5112,.F.);
#6589=ORIENTED_EDGE('',*,*,#5105,.T.);
#6590=ORIENTED_EDGE('',*,*,#5098,.T.);
#6591=ORIENTED_EDGE('',*,*,#5113,.F.);
#6592=ORIENTED_EDGE('',*,*,#5114,.T.);
#6593=ORIENTED_EDGE('',*,*,#5115,.F.);
#6594=ORIENTED_EDGE('',*,*,#5116,.F.);
#6595=ORIENTED_EDGE('',*,*,#5117,.F.);
#6596=ORIENTED_EDGE('',*,*,#5118,.F.);
#6597=ORIENTED_EDGE('',*,*,#5119,.F.);
#6598=ORIENTED_EDGE('',*,*,#5120,.F.);
#6599=ORIENTED_EDGE('',*,*,#5121,.F.);
#6600=ORIENTED_EDGE('',*,*,#5120,.T.);
#6601=ORIENTED_EDGE('',*,*,#5122,.F.);
#6602=ORIENTED_EDGE('',*,*,#5114,.F.);
#6603=ORIENTED_EDGE('',*,*,#5122,.T.);
#6604=ORIENTED_EDGE('',*,*,#5119,.T.);
#6605=ORIENTED_EDGE('',*,*,#5123,.F.);
#6606=ORIENTED_EDGE('',*,*,#5115,.T.);
#6607=ORIENTED_EDGE('',*,*,#5097,.T.);
#6608=ORIENTED_EDGE('',*,*,#5121,.T.);
#6609=ORIENTED_EDGE('',*,*,#5113,.T.);
#6610=ORIENTED_EDGE('',*,*,#5124,.F.);
#6611=ORIENTED_EDGE('',*,*,#5117,.T.);
#6612=ORIENTED_EDGE('',*,*,#5095,.T.);
#6613=ORIENTED_EDGE('',*,*,#5125,.T.);
#6614=ORIENTED_EDGE('',*,*,#5126,.T.);
#6615=ORIENTED_EDGE('',*,*,#5127,.F.);
#6616=ORIENTED_EDGE('',*,*,#5128,.F.);
#6617=ORIENTED_EDGE('',*,*,#5129,.T.);
#6618=ORIENTED_EDGE('',*,*,#5128,.T.);
#6619=ORIENTED_EDGE('',*,*,#5130,.F.);
#6620=ORIENTED_EDGE('',*,*,#5131,.F.);
#6621=ORIENTED_EDGE('',*,*,#5132,.T.);
#6622=ORIENTED_EDGE('',*,*,#5131,.T.);
#6623=ORIENTED_EDGE('',*,*,#5133,.F.);
#6624=ORIENTED_EDGE('',*,*,#5134,.F.);
#6625=ORIENTED_EDGE('',*,*,#5135,.T.);
#6626=ORIENTED_EDGE('',*,*,#5134,.T.);
#6627=ORIENTED_EDGE('',*,*,#5136,.F.);
#6628=ORIENTED_EDGE('',*,*,#5126,.F.);
#6629=ORIENTED_EDGE('',*,*,#5136,.T.);
#6630=ORIENTED_EDGE('',*,*,#5133,.T.);
#6631=ORIENTED_EDGE('',*,*,#5130,.T.);
#6632=ORIENTED_EDGE('',*,*,#5127,.T.);
#6633=ORIENTED_EDGE('',*,*,#5118,.T.);
#6634=ORIENTED_EDGE('',*,*,#5124,.T.);
#6635=ORIENTED_EDGE('',*,*,#5116,.T.);
#6636=ORIENTED_EDGE('',*,*,#5123,.T.);
#6637=ORIENTED_EDGE('',*,*,#5106,.T.);
#6638=ORIENTED_EDGE('',*,*,#5112,.T.);
#6639=ORIENTED_EDGE('',*,*,#5104,.T.);
#6640=ORIENTED_EDGE('',*,*,#5111,.T.);
#6641=ORIENTED_EDGE('',*,*,#5094,.T.);
#6642=ORIENTED_EDGE('',*,*,#5091,.T.);
#6643=ORIENTED_EDGE('',*,*,#5088,.T.);
#6644=ORIENTED_EDGE('',*,*,#5085,.T.);
#6645=ORIENTED_EDGE('',*,*,#5135,.F.);
#6646=ORIENTED_EDGE('',*,*,#5125,.F.);
#6647=ORIENTED_EDGE('',*,*,#5129,.F.);
#6648=ORIENTED_EDGE('',*,*,#5132,.F.);
#6649=ORIENTED_EDGE('',*,*,#5083,.T.);
#6650=ORIENTED_EDGE('',*,*,#5086,.T.);
#6651=ORIENTED_EDGE('',*,*,#5089,.T.);
#6652=ORIENTED_EDGE('',*,*,#5092,.T.);
#6653=ORIENTED_EDGE('',*,*,#5137,.F.);
#6654=ORIENTED_EDGE('',*,*,#5138,.T.);
#6655=ORIENTED_EDGE('',*,*,#5139,.F.);
#6656=ORIENTED_EDGE('',*,*,#5138,.F.);
#6657=ORIENTED_EDGE('',*,*,#5137,.T.);
#6658=ORIENTED_EDGE('',*,*,#5140,.T.);
#6659=ORIENTED_EDGE('',*,*,#5141,.F.);
#6660=ORIENTED_EDGE('',*,*,#5140,.F.);
#6661=ORIENTED_EDGE('',*,*,#5142,.T.);
#6662=ORIENTED_EDGE('',*,*,#5143,.T.);
#6663=ORIENTED_EDGE('',*,*,#5142,.F.);
#6664=ORIENTED_EDGE('',*,*,#5143,.F.);
#6665=ORIENTED_EDGE('',*,*,#5144,.F.);
#6666=ORIENTED_EDGE('',*,*,#5145,.T.);
#6667=ORIENTED_EDGE('',*,*,#5141,.T.);
#6668=ORIENTED_EDGE('',*,*,#5145,.F.);
#6669=ORIENTED_EDGE('',*,*,#5144,.T.);
#6670=ORIENTED_EDGE('',*,*,#5139,.T.);
#6671=ORIENTED_EDGE('',*,*,#5146,.F.);
#6672=ORIENTED_EDGE('',*,*,#5147,.T.);
#6673=ORIENTED_EDGE('',*,*,#5148,.T.);
#6674=ORIENTED_EDGE('',*,*,#5147,.F.);
#6675=ORIENTED_EDGE('',*,*,#5149,.F.);
#6676=ORIENTED_EDGE('',*,*,#5150,.T.);
#6677=ORIENTED_EDGE('',*,*,#5151,.T.);
#6678=ORIENTED_EDGE('',*,*,#5150,.F.);
#6679=ORIENTED_EDGE('',*,*,#5149,.T.);
#6680=ORIENTED_EDGE('',*,*,#5146,.T.);
#6681=ORIENTED_EDGE('',*,*,#5151,.F.);
#6682=ORIENTED_EDGE('',*,*,#5148,.F.);
#6683=ORIENTED_EDGE('',*,*,#5152,.F.);
#6684=ORIENTED_EDGE('',*,*,#5153,.T.);
#6685=ORIENTED_EDGE('',*,*,#5154,.T.);
#6686=ORIENTED_EDGE('',*,*,#5153,.F.);
#6687=ORIENTED_EDGE('',*,*,#5155,.F.);
#6688=ORIENTED_EDGE('',*,*,#5156,.T.);
#6689=ORIENTED_EDGE('',*,*,#5157,.T.);
#6690=ORIENTED_EDGE('',*,*,#5156,.F.);
#6691=ORIENTED_EDGE('',*,*,#5155,.T.);
#6692=ORIENTED_EDGE('',*,*,#5152,.T.);
#6693=ORIENTED_EDGE('',*,*,#5157,.F.);
#6694=ORIENTED_EDGE('',*,*,#5154,.F.);
#6695=ORIENTED_EDGE('',*,*,#5158,.F.);
#6696=ORIENTED_EDGE('',*,*,#5159,.T.);
#6697=ORIENTED_EDGE('',*,*,#5160,.T.);
#6698=ORIENTED_EDGE('',*,*,#5159,.F.);
#6699=ORIENTED_EDGE('',*,*,#5161,.F.);
#6700=ORIENTED_EDGE('',*,*,#5162,.T.);
#6701=ORIENTED_EDGE('',*,*,#5163,.T.);
#6702=ORIENTED_EDGE('',*,*,#5162,.F.);
#6703=ORIENTED_EDGE('',*,*,#5161,.T.);
#6704=ORIENTED_EDGE('',*,*,#5158,.T.);
#6705=ORIENTED_EDGE('',*,*,#5163,.F.);
#6706=ORIENTED_EDGE('',*,*,#5160,.F.);
#6707=ORIENTED_EDGE('',*,*,#5164,.F.);
#6708=ORIENTED_EDGE('',*,*,#5165,.T.);
#6709=ORIENTED_EDGE('',*,*,#5166,.F.);
#6710=ORIENTED_EDGE('',*,*,#5165,.F.);
#6711=ORIENTED_EDGE('',*,*,#5167,.F.);
#6712=ORIENTED_EDGE('',*,*,#5168,.T.);
#6713=ORIENTED_EDGE('',*,*,#5169,.F.);
#6714=ORIENTED_EDGE('',*,*,#5168,.F.);
#6715=ORIENTED_EDGE('',*,*,#5170,.F.);
#6716=ORIENTED_EDGE('',*,*,#5171,.T.);
#6717=ORIENTED_EDGE('',*,*,#5172,.F.);
#6718=ORIENTED_EDGE('',*,*,#5171,.F.);
#6719=ORIENTED_EDGE('',*,*,#5173,.F.);
#6720=ORIENTED_EDGE('',*,*,#5174,.T.);
#6721=ORIENTED_EDGE('',*,*,#5175,.F.);
#6722=ORIENTED_EDGE('',*,*,#5174,.F.);
#6723=ORIENTED_EDGE('',*,*,#5176,.F.);
#6724=ORIENTED_EDGE('',*,*,#5177,.T.);
#6725=ORIENTED_EDGE('',*,*,#5178,.F.);
#6726=ORIENTED_EDGE('',*,*,#5177,.F.);
#6727=ORIENTED_EDGE('',*,*,#5179,.F.);
#6728=ORIENTED_EDGE('',*,*,#5180,.T.);
#6729=ORIENTED_EDGE('',*,*,#5181,.F.);
#6730=ORIENTED_EDGE('',*,*,#5180,.F.);
#6731=ORIENTED_EDGE('',*,*,#5182,.F.);
#6732=ORIENTED_EDGE('',*,*,#5183,.T.);
#6733=ORIENTED_EDGE('',*,*,#5184,.F.);
#6734=ORIENTED_EDGE('',*,*,#5185,.F.);
#6735=ORIENTED_EDGE('',*,*,#5186,.F.);
#6736=ORIENTED_EDGE('',*,*,#5187,.F.);
#6737=ORIENTED_EDGE('',*,*,#5188,.F.);
#6738=ORIENTED_EDGE('',*,*,#5189,.F.);
#6739=ORIENTED_EDGE('',*,*,#5190,.F.);
#6740=ORIENTED_EDGE('',*,*,#5189,.T.);
#6741=ORIENTED_EDGE('',*,*,#5191,.F.);
#6742=ORIENTED_EDGE('',*,*,#5183,.F.);
#6743=ORIENTED_EDGE('',*,*,#5191,.T.);
#6744=ORIENTED_EDGE('',*,*,#5188,.T.);
#6745=ORIENTED_EDGE('',*,*,#5192,.F.);
#6746=ORIENTED_EDGE('',*,*,#5184,.T.);
#6747=ORIENTED_EDGE('',*,*,#5181,.T.);
#6748=ORIENTED_EDGE('',*,*,#5190,.T.);
#6749=ORIENTED_EDGE('',*,*,#5182,.T.);
#6750=ORIENTED_EDGE('',*,*,#5193,.F.);
#6751=ORIENTED_EDGE('',*,*,#5186,.T.);
#6752=ORIENTED_EDGE('',*,*,#5179,.T.);
#6753=ORIENTED_EDGE('',*,*,#5194,.F.);
#6754=ORIENTED_EDGE('',*,*,#5195,.T.);
#6755=ORIENTED_EDGE('',*,*,#5196,.F.);
#6756=ORIENTED_EDGE('',*,*,#5197,.F.);
#6757=ORIENTED_EDGE('',*,*,#5198,.F.);
#6758=ORIENTED_EDGE('',*,*,#5199,.F.);
#6759=ORIENTED_EDGE('',*,*,#5200,.F.);
#6760=ORIENTED_EDGE('',*,*,#5201,.F.);
#6761=ORIENTED_EDGE('',*,*,#5202,.F.);
#6762=ORIENTED_EDGE('',*,*,#5201,.T.);
#6763=ORIENTED_EDGE('',*,*,#5203,.F.);
#6764=ORIENTED_EDGE('',*,*,#5195,.F.);
#6765=ORIENTED_EDGE('',*,*,#5203,.T.);
#6766=ORIENTED_EDGE('',*,*,#5200,.T.);
#6767=ORIENTED_EDGE('',*,*,#5204,.F.);
#6768=ORIENTED_EDGE('',*,*,#5196,.T.);
#6769=ORIENTED_EDGE('',*,*,#5178,.T.);
#6770=ORIENTED_EDGE('',*,*,#5202,.T.);
#6771=ORIENTED_EDGE('',*,*,#5194,.T.);
#6772=ORIENTED_EDGE('',*,*,#5205,.F.);
#6773=ORIENTED_EDGE('',*,*,#5198,.T.);
#6774=ORIENTED_EDGE('',*,*,#5176,.T.);
#6775=ORIENTED_EDGE('',*,*,#5206,.T.);
#6776=ORIENTED_EDGE('',*,*,#5207,.T.);
#6777=ORIENTED_EDGE('',*,*,#5208,.F.);
#6778=ORIENTED_EDGE('',*,*,#5209,.F.);
#6779=ORIENTED_EDGE('',*,*,#5210,.T.);
#6780=ORIENTED_EDGE('',*,*,#5209,.T.);
#6781=ORIENTED_EDGE('',*,*,#5211,.F.);
#6782=ORIENTED_EDGE('',*,*,#5212,.F.);
#6783=ORIENTED_EDGE('',*,*,#5213,.T.);
#6784=ORIENTED_EDGE('',*,*,#5212,.T.);
#6785=ORIENTED_EDGE('',*,*,#5214,.F.);
#6786=ORIENTED_EDGE('',*,*,#5215,.F.);
#6787=ORIENTED_EDGE('',*,*,#5216,.T.);
#6788=ORIENTED_EDGE('',*,*,#5215,.T.);
#6789=ORIENTED_EDGE('',*,*,#5217,.F.);
#6790=ORIENTED_EDGE('',*,*,#5207,.F.);
#6791=ORIENTED_EDGE('',*,*,#5217,.T.);
#6792=ORIENTED_EDGE('',*,*,#5214,.T.);
#6793=ORIENTED_EDGE('',*,*,#5211,.T.);
#6794=ORIENTED_EDGE('',*,*,#5208,.T.);
#6795=ORIENTED_EDGE('',*,*,#5199,.T.);
#6796=ORIENTED_EDGE('',*,*,#5205,.T.);
#6797=ORIENTED_EDGE('',*,*,#5197,.T.);
#6798=ORIENTED_EDGE('',*,*,#5204,.T.);
#6799=ORIENTED_EDGE('',*,*,#5187,.T.);
#6800=ORIENTED_EDGE('',*,*,#5193,.T.);
#6801=ORIENTED_EDGE('',*,*,#5185,.T.);
#6802=ORIENTED_EDGE('',*,*,#5192,.T.);
#6803=ORIENTED_EDGE('',*,*,#5175,.T.);
#6804=ORIENTED_EDGE('',*,*,#5172,.T.);
#6805=ORIENTED_EDGE('',*,*,#5169,.T.);
#6806=ORIENTED_EDGE('',*,*,#5166,.T.);
#6807=ORIENTED_EDGE('',*,*,#5216,.F.);
#6808=ORIENTED_EDGE('',*,*,#5206,.F.);
#6809=ORIENTED_EDGE('',*,*,#5210,.F.);
#6810=ORIENTED_EDGE('',*,*,#5213,.F.);
#6811=ORIENTED_EDGE('',*,*,#5164,.T.);
#6812=ORIENTED_EDGE('',*,*,#5167,.T.);
#6813=ORIENTED_EDGE('',*,*,#5170,.T.);
#6814=ORIENTED_EDGE('',*,*,#5173,.T.);
#6815=ORIENTED_EDGE('',*,*,#5218,.F.);
#6816=ORIENTED_EDGE('',*,*,#5219,.T.);
#6817=ORIENTED_EDGE('',*,*,#5220,.F.);
#6818=ORIENTED_EDGE('',*,*,#5219,.F.);
#6819=ORIENTED_EDGE('',*,*,#5218,.T.);
#6820=ORIENTED_EDGE('',*,*,#5221,.T.);
#6821=ORIENTED_EDGE('',*,*,#5222,.F.);
#6822=ORIENTED_EDGE('',*,*,#5221,.F.);
#6823=ORIENTED_EDGE('',*,*,#5223,.T.);
#6824=ORIENTED_EDGE('',*,*,#5224,.T.);
#6825=ORIENTED_EDGE('',*,*,#5223,.F.);
#6826=ORIENTED_EDGE('',*,*,#5224,.F.);
#6827=ORIENTED_EDGE('',*,*,#5225,.F.);
#6828=ORIENTED_EDGE('',*,*,#5226,.T.);
#6829=ORIENTED_EDGE('',*,*,#5222,.T.);
#6830=ORIENTED_EDGE('',*,*,#5226,.F.);
#6831=ORIENTED_EDGE('',*,*,#5225,.T.);
#6832=ORIENTED_EDGE('',*,*,#5220,.T.);
#6833=ORIENTED_EDGE('',*,*,#5227,.F.);
#6834=ORIENTED_EDGE('',*,*,#5228,.T.);
#6835=ORIENTED_EDGE('',*,*,#5229,.T.);
#6836=ORIENTED_EDGE('',*,*,#5228,.F.);
#6837=ORIENTED_EDGE('',*,*,#5230,.F.);
#6838=ORIENTED_EDGE('',*,*,#5231,.T.);
#6839=ORIENTED_EDGE('',*,*,#5232,.T.);
#6840=ORIENTED_EDGE('',*,*,#5231,.F.);
#6841=ORIENTED_EDGE('',*,*,#5230,.T.);
#6842=ORIENTED_EDGE('',*,*,#5227,.T.);
#6843=ORIENTED_EDGE('',*,*,#5232,.F.);
#6844=ORIENTED_EDGE('',*,*,#5229,.F.);
#6845=ORIENTED_EDGE('',*,*,#5233,.F.);
#6846=ORIENTED_EDGE('',*,*,#5234,.T.);
#6847=ORIENTED_EDGE('',*,*,#5235,.T.);
#6848=ORIENTED_EDGE('',*,*,#5234,.F.);
#6849=ORIENTED_EDGE('',*,*,#5236,.F.);
#6850=ORIENTED_EDGE('',*,*,#5237,.T.);
#6851=ORIENTED_EDGE('',*,*,#5238,.T.);
#6852=ORIENTED_EDGE('',*,*,#5237,.F.);
#6853=ORIENTED_EDGE('',*,*,#5236,.T.);
#6854=ORIENTED_EDGE('',*,*,#5233,.T.);
#6855=ORIENTED_EDGE('',*,*,#5238,.F.);
#6856=ORIENTED_EDGE('',*,*,#5235,.F.);
#6857=ORIENTED_EDGE('',*,*,#5239,.F.);
#6858=ORIENTED_EDGE('',*,*,#5240,.T.);
#6859=ORIENTED_EDGE('',*,*,#5241,.T.);
#6860=ORIENTED_EDGE('',*,*,#5240,.F.);
#6861=ORIENTED_EDGE('',*,*,#5242,.F.);
#6862=ORIENTED_EDGE('',*,*,#5243,.T.);
#6863=ORIENTED_EDGE('',*,*,#5244,.T.);
#6864=ORIENTED_EDGE('',*,*,#5243,.F.);
#6865=ORIENTED_EDGE('',*,*,#5242,.T.);
#6866=ORIENTED_EDGE('',*,*,#5239,.T.);
#6867=ORIENTED_EDGE('',*,*,#5244,.F.);
#6868=ORIENTED_EDGE('',*,*,#5241,.F.);
#6869=ORIENTED_EDGE('',*,*,#5245,.F.);
#6870=ORIENTED_EDGE('',*,*,#5246,.T.);
#6871=ORIENTED_EDGE('',*,*,#5247,.F.);
#6872=ORIENTED_EDGE('',*,*,#5246,.F.);
#6873=ORIENTED_EDGE('',*,*,#5248,.F.);
#6874=ORIENTED_EDGE('',*,*,#5249,.T.);
#6875=ORIENTED_EDGE('',*,*,#5250,.F.);
#6876=ORIENTED_EDGE('',*,*,#5249,.F.);
#6877=ORIENTED_EDGE('',*,*,#5251,.F.);
#6878=ORIENTED_EDGE('',*,*,#5252,.T.);
#6879=ORIENTED_EDGE('',*,*,#5253,.F.);
#6880=ORIENTED_EDGE('',*,*,#5252,.F.);
#6881=ORIENTED_EDGE('',*,*,#5254,.F.);
#6882=ORIENTED_EDGE('',*,*,#5255,.T.);
#6883=ORIENTED_EDGE('',*,*,#5256,.F.);
#6884=ORIENTED_EDGE('',*,*,#5255,.F.);
#6885=ORIENTED_EDGE('',*,*,#5257,.F.);
#6886=ORIENTED_EDGE('',*,*,#5258,.T.);
#6887=ORIENTED_EDGE('',*,*,#5259,.F.);
#6888=ORIENTED_EDGE('',*,*,#5258,.F.);
#6889=ORIENTED_EDGE('',*,*,#5260,.F.);
#6890=ORIENTED_EDGE('',*,*,#5261,.T.);
#6891=ORIENTED_EDGE('',*,*,#5262,.F.);
#6892=ORIENTED_EDGE('',*,*,#5261,.F.);
#6893=ORIENTED_EDGE('',*,*,#5263,.F.);
#6894=ORIENTED_EDGE('',*,*,#5264,.T.);
#6895=ORIENTED_EDGE('',*,*,#5265,.F.);
#6896=ORIENTED_EDGE('',*,*,#5266,.F.);
#6897=ORIENTED_EDGE('',*,*,#5267,.F.);
#6898=ORIENTED_EDGE('',*,*,#5268,.F.);
#6899=ORIENTED_EDGE('',*,*,#5269,.F.);
#6900=ORIENTED_EDGE('',*,*,#5270,.F.);
#6901=ORIENTED_EDGE('',*,*,#5271,.F.);
#6902=ORIENTED_EDGE('',*,*,#5270,.T.);
#6903=ORIENTED_EDGE('',*,*,#5272,.F.);
#6904=ORIENTED_EDGE('',*,*,#5264,.F.);
#6905=ORIENTED_EDGE('',*,*,#5272,.T.);
#6906=ORIENTED_EDGE('',*,*,#5269,.T.);
#6907=ORIENTED_EDGE('',*,*,#5273,.F.);
#6908=ORIENTED_EDGE('',*,*,#5265,.T.);
#6909=ORIENTED_EDGE('',*,*,#5262,.T.);
#6910=ORIENTED_EDGE('',*,*,#5271,.T.);
#6911=ORIENTED_EDGE('',*,*,#5263,.T.);
#6912=ORIENTED_EDGE('',*,*,#5274,.F.);
#6913=ORIENTED_EDGE('',*,*,#5267,.T.);
#6914=ORIENTED_EDGE('',*,*,#5260,.T.);
#6915=ORIENTED_EDGE('',*,*,#5275,.F.);
#6916=ORIENTED_EDGE('',*,*,#5276,.T.);
#6917=ORIENTED_EDGE('',*,*,#5277,.F.);
#6918=ORIENTED_EDGE('',*,*,#5278,.F.);
#6919=ORIENTED_EDGE('',*,*,#5279,.F.);
#6920=ORIENTED_EDGE('',*,*,#5280,.F.);
#6921=ORIENTED_EDGE('',*,*,#5281,.F.);
#6922=ORIENTED_EDGE('',*,*,#5282,.F.);
#6923=ORIENTED_EDGE('',*,*,#5283,.F.);
#6924=ORIENTED_EDGE('',*,*,#5282,.T.);
#6925=ORIENTED_EDGE('',*,*,#5284,.F.);
#6926=ORIENTED_EDGE('',*,*,#5276,.F.);
#6927=ORIENTED_EDGE('',*,*,#5284,.T.);
#6928=ORIENTED_EDGE('',*,*,#5281,.T.);
#6929=ORIENTED_EDGE('',*,*,#5285,.F.);
#6930=ORIENTED_EDGE('',*,*,#5277,.T.);
#6931=ORIENTED_EDGE('',*,*,#5259,.T.);
#6932=ORIENTED_EDGE('',*,*,#5283,.T.);
#6933=ORIENTED_EDGE('',*,*,#5275,.T.);
#6934=ORIENTED_EDGE('',*,*,#5286,.F.);
#6935=ORIENTED_EDGE('',*,*,#5279,.T.);
#6936=ORIENTED_EDGE('',*,*,#5257,.T.);
#6937=ORIENTED_EDGE('',*,*,#5287,.T.);
#6938=ORIENTED_EDGE('',*,*,#5288,.T.);
#6939=ORIENTED_EDGE('',*,*,#5289,.F.);
#6940=ORIENTED_EDGE('',*,*,#5290,.F.);
#6941=ORIENTED_EDGE('',*,*,#5291,.T.);
#6942=ORIENTED_EDGE('',*,*,#5290,.T.);
#6943=ORIENTED_EDGE('',*,*,#5292,.F.);
#6944=ORIENTED_EDGE('',*,*,#5293,.F.);
#6945=ORIENTED_EDGE('',*,*,#5294,.T.);
#6946=ORIENTED_EDGE('',*,*,#5293,.T.);
#6947=ORIENTED_EDGE('',*,*,#5295,.F.);
#6948=ORIENTED_EDGE('',*,*,#5296,.F.);
#6949=ORIENTED_EDGE('',*,*,#5297,.T.);
#6950=ORIENTED_EDGE('',*,*,#5296,.T.);
#6951=ORIENTED_EDGE('',*,*,#5298,.F.);
#6952=ORIENTED_EDGE('',*,*,#5288,.F.);
#6953=ORIENTED_EDGE('',*,*,#5298,.T.);
#6954=ORIENTED_EDGE('',*,*,#5295,.T.);
#6955=ORIENTED_EDGE('',*,*,#5292,.T.);
#6956=ORIENTED_EDGE('',*,*,#5289,.T.);
#6957=ORIENTED_EDGE('',*,*,#5280,.T.);
#6958=ORIENTED_EDGE('',*,*,#5286,.T.);
#6959=ORIENTED_EDGE('',*,*,#5278,.T.);
#6960=ORIENTED_EDGE('',*,*,#5285,.T.);
#6961=ORIENTED_EDGE('',*,*,#5268,.T.);
#6962=ORIENTED_EDGE('',*,*,#5274,.T.);
#6963=ORIENTED_EDGE('',*,*,#5266,.T.);
#6964=ORIENTED_EDGE('',*,*,#5273,.T.);
#6965=ORIENTED_EDGE('',*,*,#5256,.T.);
#6966=ORIENTED_EDGE('',*,*,#5253,.T.);
#6967=ORIENTED_EDGE('',*,*,#5250,.T.);
#6968=ORIENTED_EDGE('',*,*,#5247,.T.);
#6969=ORIENTED_EDGE('',*,*,#5297,.F.);
#6970=ORIENTED_EDGE('',*,*,#5287,.F.);
#6971=ORIENTED_EDGE('',*,*,#5291,.F.);
#6972=ORIENTED_EDGE('',*,*,#5294,.F.);
#6973=ORIENTED_EDGE('',*,*,#5245,.T.);
#6974=ORIENTED_EDGE('',*,*,#5248,.T.);
#6975=ORIENTED_EDGE('',*,*,#5251,.T.);
#6976=ORIENTED_EDGE('',*,*,#5254,.T.);
#6977=ORIENTED_EDGE('',*,*,#5299,.F.);
#6978=ORIENTED_EDGE('',*,*,#5300,.T.);
#6979=ORIENTED_EDGE('',*,*,#5301,.F.);
#6980=ORIENTED_EDGE('',*,*,#5300,.F.);
#6981=ORIENTED_EDGE('',*,*,#5299,.T.);
#6982=ORIENTED_EDGE('',*,*,#5302,.T.);
#6983=ORIENTED_EDGE('',*,*,#5303,.F.);
#6984=ORIENTED_EDGE('',*,*,#5302,.F.);
#6985=ORIENTED_EDGE('',*,*,#5304,.T.);
#6986=ORIENTED_EDGE('',*,*,#5305,.T.);
#6987=ORIENTED_EDGE('',*,*,#5304,.F.);
#6988=ORIENTED_EDGE('',*,*,#5305,.F.);
#6989=ORIENTED_EDGE('',*,*,#5306,.F.);
#6990=ORIENTED_EDGE('',*,*,#5307,.T.);
#6991=ORIENTED_EDGE('',*,*,#5303,.T.);
#6992=ORIENTED_EDGE('',*,*,#5307,.F.);
#6993=ORIENTED_EDGE('',*,*,#5306,.T.);
#6994=ORIENTED_EDGE('',*,*,#5301,.T.);
#6995=ORIENTED_EDGE('',*,*,#5308,.F.);
#6996=ORIENTED_EDGE('',*,*,#5309,.T.);
#6997=ORIENTED_EDGE('',*,*,#5310,.T.);
#6998=ORIENTED_EDGE('',*,*,#5309,.F.);
#6999=ORIENTED_EDGE('',*,*,#5311,.F.);
#7000=ORIENTED_EDGE('',*,*,#5312,.T.);
#7001=ORIENTED_EDGE('',*,*,#5313,.T.);
#7002=ORIENTED_EDGE('',*,*,#5312,.F.);
#7003=ORIENTED_EDGE('',*,*,#5311,.T.);
#7004=ORIENTED_EDGE('',*,*,#5308,.T.);
#7005=ORIENTED_EDGE('',*,*,#5313,.F.);
#7006=ORIENTED_EDGE('',*,*,#5310,.F.);
#7007=ORIENTED_EDGE('',*,*,#5314,.F.);
#7008=ORIENTED_EDGE('',*,*,#5315,.T.);
#7009=ORIENTED_EDGE('',*,*,#5316,.T.);
#7010=ORIENTED_EDGE('',*,*,#5315,.F.);
#7011=ORIENTED_EDGE('',*,*,#5317,.F.);
#7012=ORIENTED_EDGE('',*,*,#5318,.T.);
#7013=ORIENTED_EDGE('',*,*,#5319,.T.);
#7014=ORIENTED_EDGE('',*,*,#5318,.F.);
#7015=ORIENTED_EDGE('',*,*,#5317,.T.);
#7016=ORIENTED_EDGE('',*,*,#5314,.T.);
#7017=ORIENTED_EDGE('',*,*,#5319,.F.);
#7018=ORIENTED_EDGE('',*,*,#5316,.F.);
#7019=ORIENTED_EDGE('',*,*,#5320,.F.);
#7020=ORIENTED_EDGE('',*,*,#5321,.T.);
#7021=ORIENTED_EDGE('',*,*,#5322,.T.);
#7022=ORIENTED_EDGE('',*,*,#5321,.F.);
#7023=ORIENTED_EDGE('',*,*,#5323,.F.);
#7024=ORIENTED_EDGE('',*,*,#5324,.T.);
#7025=ORIENTED_EDGE('',*,*,#5325,.T.);
#7026=ORIENTED_EDGE('',*,*,#5324,.F.);
#7027=ORIENTED_EDGE('',*,*,#5323,.T.);
#7028=ORIENTED_EDGE('',*,*,#5320,.T.);
#7029=ORIENTED_EDGE('',*,*,#5325,.F.);
#7030=ORIENTED_EDGE('',*,*,#5322,.F.);
#7031=ORIENTED_EDGE('',*,*,#5326,.F.);
#7032=ORIENTED_EDGE('',*,*,#5327,.T.);
#7033=ORIENTED_EDGE('',*,*,#5328,.F.);
#7034=ORIENTED_EDGE('',*,*,#5327,.F.);
#7035=ORIENTED_EDGE('',*,*,#5329,.F.);
#7036=ORIENTED_EDGE('',*,*,#5330,.T.);
#7037=ORIENTED_EDGE('',*,*,#5331,.F.);
#7038=ORIENTED_EDGE('',*,*,#5330,.F.);
#7039=ORIENTED_EDGE('',*,*,#5332,.F.);
#7040=ORIENTED_EDGE('',*,*,#5333,.T.);
#7041=ORIENTED_EDGE('',*,*,#5334,.F.);
#7042=ORIENTED_EDGE('',*,*,#5333,.F.);
#7043=ORIENTED_EDGE('',*,*,#5335,.F.);
#7044=ORIENTED_EDGE('',*,*,#5336,.T.);
#7045=ORIENTED_EDGE('',*,*,#5337,.F.);
#7046=ORIENTED_EDGE('',*,*,#5336,.F.);
#7047=ORIENTED_EDGE('',*,*,#5338,.F.);
#7048=ORIENTED_EDGE('',*,*,#5339,.T.);
#7049=ORIENTED_EDGE('',*,*,#5340,.F.);
#7050=ORIENTED_EDGE('',*,*,#5339,.F.);
#7051=ORIENTED_EDGE('',*,*,#5341,.F.);
#7052=ORIENTED_EDGE('',*,*,#5342,.T.);
#7053=ORIENTED_EDGE('',*,*,#5343,.F.);
#7054=ORIENTED_EDGE('',*,*,#5342,.F.);
#7055=ORIENTED_EDGE('',*,*,#5344,.F.);
#7056=ORIENTED_EDGE('',*,*,#5345,.T.);
#7057=ORIENTED_EDGE('',*,*,#5346,.F.);
#7058=ORIENTED_EDGE('',*,*,#5347,.F.);
#7059=ORIENTED_EDGE('',*,*,#5348,.F.);
#7060=ORIENTED_EDGE('',*,*,#5349,.F.);
#7061=ORIENTED_EDGE('',*,*,#5350,.F.);
#7062=ORIENTED_EDGE('',*,*,#5351,.F.);
#7063=ORIENTED_EDGE('',*,*,#5352,.F.);
#7064=ORIENTED_EDGE('',*,*,#5351,.T.);
#7065=ORIENTED_EDGE('',*,*,#5353,.F.);
#7066=ORIENTED_EDGE('',*,*,#5345,.F.);
#7067=ORIENTED_EDGE('',*,*,#5353,.T.);
#7068=ORIENTED_EDGE('',*,*,#5350,.T.);
#7069=ORIENTED_EDGE('',*,*,#5354,.F.);
#7070=ORIENTED_EDGE('',*,*,#5346,.T.);
#7071=ORIENTED_EDGE('',*,*,#5343,.T.);
#7072=ORIENTED_EDGE('',*,*,#5352,.T.);
#7073=ORIENTED_EDGE('',*,*,#5344,.T.);
#7074=ORIENTED_EDGE('',*,*,#5355,.F.);
#7075=ORIENTED_EDGE('',*,*,#5348,.T.);
#7076=ORIENTED_EDGE('',*,*,#5341,.T.);
#7077=ORIENTED_EDGE('',*,*,#5356,.F.);
#7078=ORIENTED_EDGE('',*,*,#5357,.T.);
#7079=ORIENTED_EDGE('',*,*,#5358,.F.);
#7080=ORIENTED_EDGE('',*,*,#5359,.F.);
#7081=ORIENTED_EDGE('',*,*,#5360,.F.);
#7082=ORIENTED_EDGE('',*,*,#5361,.F.);
#7083=ORIENTED_EDGE('',*,*,#5362,.F.);
#7084=ORIENTED_EDGE('',*,*,#5363,.F.);
#7085=ORIENTED_EDGE('',*,*,#5364,.F.);
#7086=ORIENTED_EDGE('',*,*,#5363,.T.);
#7087=ORIENTED_EDGE('',*,*,#5365,.F.);
#7088=ORIENTED_EDGE('',*,*,#5357,.F.);
#7089=ORIENTED_EDGE('',*,*,#5365,.T.);
#7090=ORIENTED_EDGE('',*,*,#5362,.T.);
#7091=ORIENTED_EDGE('',*,*,#5366,.F.);
#7092=ORIENTED_EDGE('',*,*,#5358,.T.);
#7093=ORIENTED_EDGE('',*,*,#5340,.T.);
#7094=ORIENTED_EDGE('',*,*,#5364,.T.);
#7095=ORIENTED_EDGE('',*,*,#5356,.T.);
#7096=ORIENTED_EDGE('',*,*,#5367,.F.);
#7097=ORIENTED_EDGE('',*,*,#5360,.T.);
#7098=ORIENTED_EDGE('',*,*,#5338,.T.);
#7099=ORIENTED_EDGE('',*,*,#5368,.T.);
#7100=ORIENTED_EDGE('',*,*,#5369,.T.);
#7101=ORIENTED_EDGE('',*,*,#5370,.F.);
#7102=ORIENTED_EDGE('',*,*,#5371,.F.);
#7103=ORIENTED_EDGE('',*,*,#5372,.T.);
#7104=ORIENTED_EDGE('',*,*,#5371,.T.);
#7105=ORIENTED_EDGE('',*,*,#5373,.F.);
#7106=ORIENTED_EDGE('',*,*,#5374,.F.);
#7107=ORIENTED_EDGE('',*,*,#5375,.T.);
#7108=ORIENTED_EDGE('',*,*,#5374,.T.);
#7109=ORIENTED_EDGE('',*,*,#5376,.F.);
#7110=ORIENTED_EDGE('',*,*,#5377,.F.);
#7111=ORIENTED_EDGE('',*,*,#5378,.T.);
#7112=ORIENTED_EDGE('',*,*,#5377,.T.);
#7113=ORIENTED_EDGE('',*,*,#5379,.F.);
#7114=ORIENTED_EDGE('',*,*,#5369,.F.);
#7115=ORIENTED_EDGE('',*,*,#5379,.T.);
#7116=ORIENTED_EDGE('',*,*,#5376,.T.);
#7117=ORIENTED_EDGE('',*,*,#5373,.T.);
#7118=ORIENTED_EDGE('',*,*,#5370,.T.);
#7119=ORIENTED_EDGE('',*,*,#5361,.T.);
#7120=ORIENTED_EDGE('',*,*,#5367,.T.);
#7121=ORIENTED_EDGE('',*,*,#5359,.T.);
#7122=ORIENTED_EDGE('',*,*,#5366,.T.);
#7123=ORIENTED_EDGE('',*,*,#5349,.T.);
#7124=ORIENTED_EDGE('',*,*,#5355,.T.);
#7125=ORIENTED_EDGE('',*,*,#5347,.T.);
#7126=ORIENTED_EDGE('',*,*,#5354,.T.);
#7127=ORIENTED_EDGE('',*,*,#5337,.T.);
#7128=ORIENTED_EDGE('',*,*,#5334,.T.);
#7129=ORIENTED_EDGE('',*,*,#5331,.T.);
#7130=ORIENTED_EDGE('',*,*,#5328,.T.);
#7131=ORIENTED_EDGE('',*,*,#5378,.F.);
#7132=ORIENTED_EDGE('',*,*,#5368,.F.);
#7133=ORIENTED_EDGE('',*,*,#5372,.F.);
#7134=ORIENTED_EDGE('',*,*,#5375,.F.);
#7135=ORIENTED_EDGE('',*,*,#5326,.T.);
#7136=ORIENTED_EDGE('',*,*,#5329,.T.);
#7137=ORIENTED_EDGE('',*,*,#5332,.T.);
#7138=ORIENTED_EDGE('',*,*,#5335,.T.);
#7139=ORIENTED_EDGE('',*,*,#5380,.F.);
#7140=ORIENTED_EDGE('',*,*,#5381,.T.);
#7141=ORIENTED_EDGE('',*,*,#5382,.F.);
#7142=ORIENTED_EDGE('',*,*,#5381,.F.);
#7143=ORIENTED_EDGE('',*,*,#5380,.T.);
#7144=ORIENTED_EDGE('',*,*,#5383,.T.);
#7145=ORIENTED_EDGE('',*,*,#5384,.F.);
#7146=ORIENTED_EDGE('',*,*,#5383,.F.);
#7147=ORIENTED_EDGE('',*,*,#5385,.T.);
#7148=ORIENTED_EDGE('',*,*,#5386,.T.);
#7149=ORIENTED_EDGE('',*,*,#5385,.F.);
#7150=ORIENTED_EDGE('',*,*,#5386,.F.);
#7151=ORIENTED_EDGE('',*,*,#5387,.F.);
#7152=ORIENTED_EDGE('',*,*,#5388,.T.);
#7153=ORIENTED_EDGE('',*,*,#5384,.T.);
#7154=ORIENTED_EDGE('',*,*,#5388,.F.);
#7155=ORIENTED_EDGE('',*,*,#5387,.T.);
#7156=ORIENTED_EDGE('',*,*,#5382,.T.);
#7157=ORIENTED_EDGE('',*,*,#5389,.F.);
#7158=ORIENTED_EDGE('',*,*,#5390,.T.);
#7159=ORIENTED_EDGE('',*,*,#5391,.T.);
#7160=ORIENTED_EDGE('',*,*,#5390,.F.);
#7161=ORIENTED_EDGE('',*,*,#5392,.F.);
#7162=ORIENTED_EDGE('',*,*,#5393,.T.);
#7163=ORIENTED_EDGE('',*,*,#5394,.T.);
#7164=ORIENTED_EDGE('',*,*,#5393,.F.);
#7165=ORIENTED_EDGE('',*,*,#5392,.T.);
#7166=ORIENTED_EDGE('',*,*,#5389,.T.);
#7167=ORIENTED_EDGE('',*,*,#5394,.F.);
#7168=ORIENTED_EDGE('',*,*,#5391,.F.);
#7169=ORIENTED_EDGE('',*,*,#5395,.F.);
#7170=ORIENTED_EDGE('',*,*,#5396,.T.);
#7171=ORIENTED_EDGE('',*,*,#5397,.T.);
#7172=ORIENTED_EDGE('',*,*,#5396,.F.);
#7173=ORIENTED_EDGE('',*,*,#5398,.F.);
#7174=ORIENTED_EDGE('',*,*,#5399,.T.);
#7175=ORIENTED_EDGE('',*,*,#5400,.T.);
#7176=ORIENTED_EDGE('',*,*,#5399,.F.);
#7177=ORIENTED_EDGE('',*,*,#5398,.T.);
#7178=ORIENTED_EDGE('',*,*,#5395,.T.);
#7179=ORIENTED_EDGE('',*,*,#5400,.F.);
#7180=ORIENTED_EDGE('',*,*,#5397,.F.);
#7181=ORIENTED_EDGE('',*,*,#5401,.F.);
#7182=ORIENTED_EDGE('',*,*,#5402,.T.);
#7183=ORIENTED_EDGE('',*,*,#5403,.T.);
#7184=ORIENTED_EDGE('',*,*,#5402,.F.);
#7185=ORIENTED_EDGE('',*,*,#5404,.F.);
#7186=ORIENTED_EDGE('',*,*,#5405,.T.);
#7187=ORIENTED_EDGE('',*,*,#5406,.T.);
#7188=ORIENTED_EDGE('',*,*,#5405,.F.);
#7189=ORIENTED_EDGE('',*,*,#5404,.T.);
#7190=ORIENTED_EDGE('',*,*,#5401,.T.);
#7191=ORIENTED_EDGE('',*,*,#5406,.F.);
#7192=ORIENTED_EDGE('',*,*,#5403,.F.);
#7193=ORIENTED_EDGE('',*,*,#5407,.T.);
#7194=ORIENTED_EDGE('',*,*,#5408,.T.);
#7195=ORIENTED_EDGE('',*,*,#5409,.T.);
#7196=ORIENTED_EDGE('',*,*,#5410,.F.);
#7197=ORIENTED_EDGE('',*,*,#5411,.T.);
#7198=ORIENTED_EDGE('',*,*,#5412,.T.);
#7199=ORIENTED_EDGE('',*,*,#5413,.T.);
#7200=ORIENTED_EDGE('',*,*,#5408,.F.);
#7201=ORIENTED_EDGE('',*,*,#5414,.T.);
#7202=ORIENTED_EDGE('',*,*,#5415,.T.);
#7203=ORIENTED_EDGE('',*,*,#5416,.T.);
#7204=ORIENTED_EDGE('',*,*,#5412,.F.);
#7205=ORIENTED_EDGE('',*,*,#5417,.T.);
#7206=ORIENTED_EDGE('',*,*,#5418,.T.);
#7207=ORIENTED_EDGE('',*,*,#5419,.T.);
#7208=ORIENTED_EDGE('',*,*,#5415,.F.);
#7209=ORIENTED_EDGE('',*,*,#5420,.T.);
#7210=ORIENTED_EDGE('',*,*,#5421,.T.);
#7211=ORIENTED_EDGE('',*,*,#5422,.T.);
#7212=ORIENTED_EDGE('',*,*,#5418,.F.);
#7213=ORIENTED_EDGE('',*,*,#5423,.T.);
#7214=ORIENTED_EDGE('',*,*,#5410,.T.);
#7215=ORIENTED_EDGE('',*,*,#5424,.T.);
#7216=ORIENTED_EDGE('',*,*,#5421,.F.);
#7217=ORIENTED_EDGE('',*,*,#5423,.F.);
#7218=ORIENTED_EDGE('',*,*,#5420,.F.);
#7219=ORIENTED_EDGE('',*,*,#5417,.F.);
#7220=ORIENTED_EDGE('',*,*,#5414,.F.);
#7221=ORIENTED_EDGE('',*,*,#5411,.F.);
#7222=ORIENTED_EDGE('',*,*,#5407,.F.);
#7223=ORIENTED_EDGE('',*,*,#5424,.F.);
#7224=ORIENTED_EDGE('',*,*,#5409,.F.);
#7225=ORIENTED_EDGE('',*,*,#5413,.F.);
#7226=ORIENTED_EDGE('',*,*,#5416,.F.);
#7227=ORIENTED_EDGE('',*,*,#5419,.F.);
#7228=ORIENTED_EDGE('',*,*,#5422,.F.);
#7229=ORIENTED_EDGE('',*,*,#5425,.F.);
#7230=ORIENTED_EDGE('',*,*,#5426,.F.);
#7231=ORIENTED_EDGE('',*,*,#5427,.F.);
#7232=ORIENTED_EDGE('',*,*,#5428,.T.);
#7233=ORIENTED_EDGE('',*,*,#5426,.T.);
#7234=ORIENTED_EDGE('',*,*,#5428,.F.);
#7235=ORIENTED_EDGE('',*,*,#5429,.F.);
#7236=ORIENTED_EDGE('',*,*,#5430,.T.);
#7237=ORIENTED_EDGE('',*,*,#5427,.T.);
#7238=ORIENTED_EDGE('',*,*,#5430,.F.);
#7239=ORIENTED_EDGE('',*,*,#5431,.F.);
#7240=ORIENTED_EDGE('',*,*,#5432,.T.);
#7241=ORIENTED_EDGE('',*,*,#5429,.T.);
#7242=ORIENTED_EDGE('',*,*,#5432,.F.);
#7243=ORIENTED_EDGE('',*,*,#5431,.T.);
#7244=ORIENTED_EDGE('',*,*,#5433,.F.);
#7245=ORIENTED_EDGE('',*,*,#5434,.F.);
#7246=ORIENTED_EDGE('',*,*,#5435,.T.);
#7247=ORIENTED_EDGE('',*,*,#5433,.T.);
#7248=ORIENTED_EDGE('',*,*,#5435,.F.);
#7249=ORIENTED_EDGE('',*,*,#5425,.T.);
#7250=ORIENTED_EDGE('',*,*,#5436,.T.);
#7251=ORIENTED_EDGE('',*,*,#5434,.T.);
#7252=ORIENTED_EDGE('',*,*,#5436,.F.);
#7253=ORIENTED_EDGE('',*,*,#5437,.T.);
#7254=ORIENTED_EDGE('',*,*,#5438,.T.);
#7255=ORIENTED_EDGE('',*,*,#5439,.T.);
#7256=ORIENTED_EDGE('',*,*,#5440,.F.);
#7257=ORIENTED_EDGE('',*,*,#5441,.T.);
#7258=ORIENTED_EDGE('',*,*,#5442,.T.);
#7259=ORIENTED_EDGE('',*,*,#5443,.T.);
#7260=ORIENTED_EDGE('',*,*,#5438,.F.);
#7261=ORIENTED_EDGE('',*,*,#5444,.T.);
#7262=ORIENTED_EDGE('',*,*,#5445,.T.);
#7263=ORIENTED_EDGE('',*,*,#5446,.T.);
#7264=ORIENTED_EDGE('',*,*,#5442,.F.);
#7265=ORIENTED_EDGE('',*,*,#5447,.T.);
#7266=ORIENTED_EDGE('',*,*,#5448,.T.);
#7267=ORIENTED_EDGE('',*,*,#5449,.T.);
#7268=ORIENTED_EDGE('',*,*,#5445,.F.);
#7269=ORIENTED_EDGE('',*,*,#5450,.T.);
#7270=ORIENTED_EDGE('',*,*,#5451,.T.);
#7271=ORIENTED_EDGE('',*,*,#5452,.T.);
#7272=ORIENTED_EDGE('',*,*,#5448,.F.);
#7273=ORIENTED_EDGE('',*,*,#5453,.T.);
#7274=ORIENTED_EDGE('',*,*,#5440,.T.);
#7275=ORIENTED_EDGE('',*,*,#5454,.T.);
#7276=ORIENTED_EDGE('',*,*,#5451,.F.);
#7277=ORIENTED_EDGE('',*,*,#5453,.F.);
#7278=ORIENTED_EDGE('',*,*,#5450,.F.);
#7279=ORIENTED_EDGE('',*,*,#5447,.F.);
#7280=ORIENTED_EDGE('',*,*,#5444,.F.);
#7281=ORIENTED_EDGE('',*,*,#5441,.F.);
#7282=ORIENTED_EDGE('',*,*,#5437,.F.);
#7283=ORIENTED_EDGE('',*,*,#5454,.F.);
#7284=ORIENTED_EDGE('',*,*,#5439,.F.);
#7285=ORIENTED_EDGE('',*,*,#5443,.F.);
#7286=ORIENTED_EDGE('',*,*,#5446,.F.);
#7287=ORIENTED_EDGE('',*,*,#5449,.F.);
#7288=ORIENTED_EDGE('',*,*,#5452,.F.);
#7289=ORIENTED_EDGE('',*,*,#5455,.F.);
#7290=ORIENTED_EDGE('',*,*,#5456,.F.);
#7291=ORIENTED_EDGE('',*,*,#5457,.F.);
#7292=ORIENTED_EDGE('',*,*,#5458,.T.);
#7293=ORIENTED_EDGE('',*,*,#5456,.T.);
#7294=ORIENTED_EDGE('',*,*,#5458,.F.);
#7295=ORIENTED_EDGE('',*,*,#5459,.F.);
#7296=ORIENTED_EDGE('',*,*,#5460,.T.);
#7297=ORIENTED_EDGE('',*,*,#5457,.T.);
#7298=ORIENTED_EDGE('',*,*,#5460,.F.);
#7299=ORIENTED_EDGE('',*,*,#5461,.F.);
#7300=ORIENTED_EDGE('',*,*,#5462,.T.);
#7301=ORIENTED_EDGE('',*,*,#5459,.T.);
#7302=ORIENTED_EDGE('',*,*,#5462,.F.);
#7303=ORIENTED_EDGE('',*,*,#5461,.T.);
#7304=ORIENTED_EDGE('',*,*,#5463,.F.);
#7305=ORIENTED_EDGE('',*,*,#5464,.F.);
#7306=ORIENTED_EDGE('',*,*,#5465,.T.);
#7307=ORIENTED_EDGE('',*,*,#5463,.T.);
#7308=ORIENTED_EDGE('',*,*,#5465,.F.);
#7309=ORIENTED_EDGE('',*,*,#5455,.T.);
#7310=ORIENTED_EDGE('',*,*,#5466,.T.);
#7311=ORIENTED_EDGE('',*,*,#5464,.T.);
#7312=ORIENTED_EDGE('',*,*,#5466,.F.);
#7313=ORIENTED_EDGE('',*,*,#5467,.F.);
#7314=ORIENTED_EDGE('',*,*,#5468,.T.);
#7315=ORIENTED_EDGE('',*,*,#5469,.T.);
#7316=ORIENTED_EDGE('',*,*,#5468,.F.);
#7317=ORIENTED_EDGE('',*,*,#5470,.F.);
#7318=ORIENTED_EDGE('',*,*,#5471,.T.);
#7319=ORIENTED_EDGE('',*,*,#5472,.T.);
#7320=ORIENTED_EDGE('',*,*,#5471,.F.);
#7321=ORIENTED_EDGE('',*,*,#5470,.T.);
#7322=ORIENTED_EDGE('',*,*,#5467,.T.);
#7323=ORIENTED_EDGE('',*,*,#5472,.F.);
#7324=ORIENTED_EDGE('',*,*,#5469,.F.);
#7325=ORIENTED_EDGE('',*,*,#5473,.F.);
#7326=ORIENTED_EDGE('',*,*,#5474,.T.);
#7327=ORIENTED_EDGE('',*,*,#5475,.T.);
#7328=ORIENTED_EDGE('',*,*,#5474,.F.);
#7329=ORIENTED_EDGE('',*,*,#5476,.F.);
#7330=ORIENTED_EDGE('',*,*,#5477,.T.);
#7331=ORIENTED_EDGE('',*,*,#5478,.T.);
#7332=ORIENTED_EDGE('',*,*,#5477,.F.);
#7333=ORIENTED_EDGE('',*,*,#5476,.T.);
#7334=ORIENTED_EDGE('',*,*,#5473,.T.);
#7335=ORIENTED_EDGE('',*,*,#5478,.F.);
#7336=ORIENTED_EDGE('',*,*,#5475,.F.);
#7337=ORIENTED_EDGE('',*,*,#5479,.F.);
#7338=ORIENTED_EDGE('',*,*,#5480,.T.);
#7339=ORIENTED_EDGE('',*,*,#5481,.T.);
#7340=ORIENTED_EDGE('',*,*,#5480,.F.);
#7341=ORIENTED_EDGE('',*,*,#5482,.F.);
#7342=ORIENTED_EDGE('',*,*,#5483,.T.);
#7343=ORIENTED_EDGE('',*,*,#5484,.T.);
#7344=ORIENTED_EDGE('',*,*,#5483,.F.);
#7345=ORIENTED_EDGE('',*,*,#5482,.T.);
#7346=ORIENTED_EDGE('',*,*,#5479,.T.);
#7347=ORIENTED_EDGE('',*,*,#5484,.F.);
#7348=ORIENTED_EDGE('',*,*,#5481,.F.);
#7349=ORIENTED_EDGE('',*,*,#5485,.F.);
#7350=ORIENTED_EDGE('',*,*,#5486,.T.);
#7351=ORIENTED_EDGE('',*,*,#5487,.T.);
#7352=ORIENTED_EDGE('',*,*,#5486,.F.);
#7353=ORIENTED_EDGE('',*,*,#5488,.F.);
#7354=ORIENTED_EDGE('',*,*,#5489,.T.);
#7355=ORIENTED_EDGE('',*,*,#5490,.T.);
#7356=ORIENTED_EDGE('',*,*,#5489,.F.);
#7357=ORIENTED_EDGE('',*,*,#5488,.T.);
#7358=ORIENTED_EDGE('',*,*,#5485,.T.);
#7359=ORIENTED_EDGE('',*,*,#5490,.F.);
#7360=ORIENTED_EDGE('',*,*,#5487,.F.);
#7361=ORIENTED_EDGE('',*,*,#5491,.F.);
#7362=ORIENTED_EDGE('',*,*,#5492,.T.);
#7363=ORIENTED_EDGE('',*,*,#5493,.T.);
#7364=ORIENTED_EDGE('',*,*,#5492,.F.);
#7365=ORIENTED_EDGE('',*,*,#5494,.F.);
#7366=ORIENTED_EDGE('',*,*,#5495,.T.);
#7367=ORIENTED_EDGE('',*,*,#5496,.T.);
#7368=ORIENTED_EDGE('',*,*,#5495,.F.);
#7369=ORIENTED_EDGE('',*,*,#5494,.T.);
#7370=ORIENTED_EDGE('',*,*,#5491,.T.);
#7371=ORIENTED_EDGE('',*,*,#5496,.F.);
#7372=ORIENTED_EDGE('',*,*,#5493,.F.);
#7373=ORIENTED_EDGE('',*,*,#5497,.F.);
#7374=ORIENTED_EDGE('',*,*,#5498,.T.);
#7375=ORIENTED_EDGE('',*,*,#5499,.T.);
#7376=ORIENTED_EDGE('',*,*,#5498,.F.);
#7377=ORIENTED_EDGE('',*,*,#5500,.F.);
#7378=ORIENTED_EDGE('',*,*,#5501,.T.);
#7379=ORIENTED_EDGE('',*,*,#5502,.T.);
#7380=ORIENTED_EDGE('',*,*,#5501,.F.);
#7381=ORIENTED_EDGE('',*,*,#5500,.T.);
#7382=ORIENTED_EDGE('',*,*,#5497,.T.);
#7383=ORIENTED_EDGE('',*,*,#5502,.F.);
#7384=ORIENTED_EDGE('',*,*,#5499,.F.);
#7385=ORIENTED_EDGE('',*,*,#5503,.F.);
#7386=ORIENTED_EDGE('',*,*,#5504,.T.);
#7387=ORIENTED_EDGE('',*,*,#5505,.T.);
#7388=ORIENTED_EDGE('',*,*,#5504,.F.);
#7389=ORIENTED_EDGE('',*,*,#5506,.F.);
#7390=ORIENTED_EDGE('',*,*,#5507,.T.);
#7391=ORIENTED_EDGE('',*,*,#5508,.T.);
#7392=ORIENTED_EDGE('',*,*,#5507,.F.);
#7393=ORIENTED_EDGE('',*,*,#5506,.T.);
#7394=ORIENTED_EDGE('',*,*,#5503,.T.);
#7395=ORIENTED_EDGE('',*,*,#5508,.F.);
#7396=ORIENTED_EDGE('',*,*,#5505,.F.);
#7397=ORIENTED_EDGE('',*,*,#5509,.F.);
#7398=ORIENTED_EDGE('',*,*,#5510,.T.);
#7399=ORIENTED_EDGE('',*,*,#5511,.T.);
#7400=ORIENTED_EDGE('',*,*,#5510,.F.);
#7401=ORIENTED_EDGE('',*,*,#5512,.F.);
#7402=ORIENTED_EDGE('',*,*,#5513,.T.);
#7403=ORIENTED_EDGE('',*,*,#5514,.T.);
#7404=ORIENTED_EDGE('',*,*,#5513,.F.);
#7405=ORIENTED_EDGE('',*,*,#5512,.T.);
#7406=ORIENTED_EDGE('',*,*,#5509,.T.);
#7407=ORIENTED_EDGE('',*,*,#5514,.F.);
#7408=ORIENTED_EDGE('',*,*,#5511,.F.);
#7409=ORIENTED_EDGE('',*,*,#5515,.F.);
#7410=ORIENTED_EDGE('',*,*,#5516,.T.);
#7411=ORIENTED_EDGE('',*,*,#5517,.T.);
#7412=ORIENTED_EDGE('',*,*,#5516,.F.);
#7413=ORIENTED_EDGE('',*,*,#5518,.F.);
#7414=ORIENTED_EDGE('',*,*,#5519,.T.);
#7415=ORIENTED_EDGE('',*,*,#5520,.T.);
#7416=ORIENTED_EDGE('',*,*,#5519,.F.);
#7417=ORIENTED_EDGE('',*,*,#5518,.T.);
#7418=ORIENTED_EDGE('',*,*,#5515,.T.);
#7419=ORIENTED_EDGE('',*,*,#5520,.F.);
#7420=ORIENTED_EDGE('',*,*,#5517,.F.);
#7421=ORIENTED_EDGE('',*,*,#5521,.F.);
#7422=ORIENTED_EDGE('',*,*,#5522,.T.);
#7423=ORIENTED_EDGE('',*,*,#5523,.T.);
#7424=ORIENTED_EDGE('',*,*,#5522,.F.);
#7425=ORIENTED_EDGE('',*,*,#5524,.F.);
#7426=ORIENTED_EDGE('',*,*,#5525,.T.);
#7427=ORIENTED_EDGE('',*,*,#5526,.T.);
#7428=ORIENTED_EDGE('',*,*,#5525,.F.);
#7429=ORIENTED_EDGE('',*,*,#5524,.T.);
#7430=ORIENTED_EDGE('',*,*,#5521,.T.);
#7431=ORIENTED_EDGE('',*,*,#5526,.F.);
#7432=ORIENTED_EDGE('',*,*,#5523,.F.);
#7433=ORIENTED_EDGE('',*,*,#5527,.F.);
#7434=ORIENTED_EDGE('',*,*,#5528,.T.);
#7435=ORIENTED_EDGE('',*,*,#5529,.T.);
#7436=ORIENTED_EDGE('',*,*,#5528,.F.);
#7437=ORIENTED_EDGE('',*,*,#5530,.F.);
#7438=ORIENTED_EDGE('',*,*,#5531,.T.);
#7439=ORIENTED_EDGE('',*,*,#5532,.T.);
#7440=ORIENTED_EDGE('',*,*,#5531,.F.);
#7441=ORIENTED_EDGE('',*,*,#5530,.T.);
#7442=ORIENTED_EDGE('',*,*,#5527,.T.);
#7443=ORIENTED_EDGE('',*,*,#5532,.F.);
#7444=ORIENTED_EDGE('',*,*,#5529,.F.);
#7445=ORIENTED_EDGE('',*,*,#5533,.F.);
#7446=ORIENTED_EDGE('',*,*,#5534,.T.);
#7447=ORIENTED_EDGE('',*,*,#5535,.T.);
#7448=ORIENTED_EDGE('',*,*,#5534,.F.);
#7449=ORIENTED_EDGE('',*,*,#5536,.F.);
#7450=ORIENTED_EDGE('',*,*,#5537,.T.);
#7451=ORIENTED_EDGE('',*,*,#5538,.T.);
#7452=ORIENTED_EDGE('',*,*,#5537,.F.);
#7453=ORIENTED_EDGE('',*,*,#5536,.T.);
#7454=ORIENTED_EDGE('',*,*,#5533,.T.);
#7455=ORIENTED_EDGE('',*,*,#5538,.F.);
#7456=ORIENTED_EDGE('',*,*,#5535,.F.);
#7457=ORIENTED_EDGE('',*,*,#5539,.F.);
#7458=ORIENTED_EDGE('',*,*,#5540,.F.);
#7459=ORIENTED_EDGE('',*,*,#5541,.T.);
#7460=ORIENTED_EDGE('',*,*,#5542,.F.);
#7461=ORIENTED_EDGE('',*,*,#5543,.F.);
#7462=ORIENTED_EDGE('',*,*,#5541,.F.);
#7463=ORIENTED_EDGE('',*,*,#5542,.T.);
#7464=ORIENTED_EDGE('',*,*,#5543,.T.);
#7465=ORIENTED_EDGE('',*,*,#5544,.T.);
#7466=ORIENTED_EDGE('',*,*,#5545,.T.);
#7467=ORIENTED_EDGE('',*,*,#5544,.F.);
#7468=ORIENTED_EDGE('',*,*,#5546,.T.);
#7469=ORIENTED_EDGE('',*,*,#5547,.T.);
#7470=ORIENTED_EDGE('',*,*,#5548,.F.);
#7471=ORIENTED_EDGE('',*,*,#5547,.F.);
#7472=ORIENTED_EDGE('',*,*,#5548,.T.);
#7473=ORIENTED_EDGE('',*,*,#5549,.T.);
#7474=ORIENTED_EDGE('',*,*,#5550,.F.);
#7475=ORIENTED_EDGE('',*,*,#5549,.F.);
#7476=ORIENTED_EDGE('',*,*,#5545,.F.);
#7477=ORIENTED_EDGE('',*,*,#5550,.T.);
#7478=ORIENTED_EDGE('',*,*,#5551,.F.);
#7479=ORIENTED_EDGE('',*,*,#5552,.T.);
#7480=ORIENTED_EDGE('',*,*,#5539,.T.);
#7481=ORIENTED_EDGE('',*,*,#5540,.T.);
#7482=ORIENTED_EDGE('',*,*,#5552,.F.);
#7483=ORIENTED_EDGE('',*,*,#5551,.T.);
#7484=ORIENTED_EDGE('',*,*,#5553,.F.);
#7485=ORIENTED_EDGE('',*,*,#5553,.T.);
#7486=ORIENTED_EDGE('',*,*,#5554,.T.);
#7487=ORIENTED_EDGE('',*,*,#5546,.F.);
#7488=ORIENTED_EDGE('',*,*,#5554,.F.);
#7489=ORIENTED_EDGE('',*,*,#5555,.F.);
#7490=ORIENTED_EDGE('',*,*,#5556,.F.);
#7491=ORIENTED_EDGE('',*,*,#5557,.T.);
#7492=ORIENTED_EDGE('',*,*,#5558,.F.);
#7493=ORIENTED_EDGE('',*,*,#5559,.F.);
#7494=ORIENTED_EDGE('',*,*,#5557,.F.);
#7495=ORIENTED_EDGE('',*,*,#5560,.T.);
#7496=ORIENTED_EDGE('',*,*,#5561,.T.);
#7497=ORIENTED_EDGE('',*,*,#5558,.T.);
#7498=ORIENTED_EDGE('',*,*,#5559,.T.);
#7499=ORIENTED_EDGE('',*,*,#5561,.F.);
#7500=ORIENTED_EDGE('',*,*,#5562,.F.);
#7501=ORIENTED_EDGE('',*,*,#5563,.T.);
#7502=ORIENTED_EDGE('',*,*,#5564,.F.);
#7503=ORIENTED_EDGE('',*,*,#5565,.T.);
#7504=ORIENTED_EDGE('',*,*,#5562,.T.);
#7505=ORIENTED_EDGE('',*,*,#5565,.F.);
#7506=ORIENTED_EDGE('',*,*,#5566,.F.);
#7507=ORIENTED_EDGE('',*,*,#5567,.T.);
#7508=ORIENTED_EDGE('',*,*,#5564,.T.);
#7509=ORIENTED_EDGE('',*,*,#5567,.F.);
#7510=ORIENTED_EDGE('',*,*,#5568,.F.);
#7511=ORIENTED_EDGE('',*,*,#5569,.T.);
#7512=ORIENTED_EDGE('',*,*,#5566,.T.);
#7513=ORIENTED_EDGE('',*,*,#5569,.F.);
#7514=ORIENTED_EDGE('',*,*,#5568,.T.);
#7515=ORIENTED_EDGE('',*,*,#5560,.F.);
#7516=ORIENTED_EDGE('',*,*,#5555,.T.);
#7517=ORIENTED_EDGE('',*,*,#5556,.T.);
#7518=ORIENTED_EDGE('',*,*,#5570,.T.);
#7519=ORIENTED_EDGE('',*,*,#5563,.F.);
#7520=ORIENTED_EDGE('',*,*,#5570,.F.);
#7521=ORIENTED_EDGE('',*,*,#5571,.T.);
#7522=ORIENTED_EDGE('',*,*,#5571,.F.);
#7523=ORIENTED_EDGE('',*,*,#5572,.T.);
#7524=ORIENTED_EDGE('',*,*,#5572,.F.);
#7525=ORIENTED_EDGE('',*,*,#5573,.T.);
#7526=ORIENTED_EDGE('',*,*,#5573,.F.);
#7527=ORIENTED_EDGE('',*,*,#5574,.T.);
#7528=ORIENTED_EDGE('',*,*,#5574,.F.);
#7529=ORIENTED_EDGE('',*,*,#5575,.T.);
#7530=ORIENTED_EDGE('',*,*,#5575,.F.);
#7531=ORIENTED_EDGE('',*,*,#5576,.T.);
#7532=ORIENTED_EDGE('',*,*,#5576,.F.);
#7533=ORIENTED_EDGE('',*,*,#5577,.T.);
#7534=ORIENTED_EDGE('',*,*,#5577,.F.);
#7535=ORIENTED_EDGE('',*,*,#5578,.T.);
#7536=ORIENTED_EDGE('',*,*,#5578,.F.);
#7537=ORIENTED_EDGE('',*,*,#5579,.F.);
#7538=ORIENTED_EDGE('',*,*,#5580,.F.);
#7539=ORIENTED_EDGE('',*,*,#5581,.F.);
#7540=ORIENTED_EDGE('',*,*,#5582,.F.);
#7541=ORIENTED_EDGE('',*,*,#5581,.T.);
#7542=ORIENTED_EDGE('',*,*,#5583,.F.);
#7543=ORIENTED_EDGE('',*,*,#5584,.T.);
#7544=ORIENTED_EDGE('',*,*,#5585,.F.);
#7545=ORIENTED_EDGE('',*,*,#5586,.T.);
#7546=ORIENTED_EDGE('',*,*,#5587,.F.);
#7547=ORIENTED_EDGE('',*,*,#5588,.T.);
#7548=ORIENTED_EDGE('',*,*,#5589,.T.);
#7549=ORIENTED_EDGE('',*,*,#5590,.F.);
#7550=ORIENTED_EDGE('',*,*,#5589,.F.);
#7551=ORIENTED_EDGE('',*,*,#5591,.T.);
#7552=ORIENTED_EDGE('',*,*,#5592,.F.);
#7553=ORIENTED_EDGE('',*,*,#5593,.T.);
#7554=ORIENTED_EDGE('',*,*,#5594,.F.);
#7555=ORIENTED_EDGE('',*,*,#5595,.T.);
#7556=ORIENTED_EDGE('',*,*,#5596,.F.);
#7557=ORIENTED_EDGE('',*,*,#5597,.T.);
#7558=ORIENTED_EDGE('',*,*,#5598,.F.);
#7559=ORIENTED_EDGE('',*,*,#5599,.T.);
#7560=ORIENTED_EDGE('',*,*,#5600,.F.);
#7561=ORIENTED_EDGE('',*,*,#5580,.T.);
#7562=ORIENTED_EDGE('',*,*,#5601,.T.);
#7563=ORIENTED_EDGE('',*,*,#5602,.T.);
#7564=ORIENTED_EDGE('',*,*,#5583,.T.);
#7565=ORIENTED_EDGE('',*,*,#5603,.F.);
#7566=ORIENTED_EDGE('',*,*,#5604,.F.);
#7567=ORIENTED_EDGE('',*,*,#5584,.F.);
#7568=ORIENTED_EDGE('',*,*,#5602,.F.);
#7569=ORIENTED_EDGE('',*,*,#5604,.T.);
#7570=ORIENTED_EDGE('',*,*,#5605,.T.);
#7571=ORIENTED_EDGE('',*,*,#5606,.T.);
#7572=ORIENTED_EDGE('',*,*,#5585,.T.);
#7573=ORIENTED_EDGE('',*,*,#5607,.F.);
#7574=ORIENTED_EDGE('',*,*,#5608,.F.);
#7575=ORIENTED_EDGE('',*,*,#5586,.F.);
#7576=ORIENTED_EDGE('',*,*,#5606,.F.);
#7577=ORIENTED_EDGE('',*,*,#5608,.T.);
#7578=ORIENTED_EDGE('',*,*,#5609,.T.);
#7579=ORIENTED_EDGE('',*,*,#5610,.T.);
#7580=ORIENTED_EDGE('',*,*,#5587,.T.);
#7581=ORIENTED_EDGE('',*,*,#5611,.F.);
#7582=ORIENTED_EDGE('',*,*,#5612,.F.);
#7583=ORIENTED_EDGE('',*,*,#5591,.F.);
#7584=ORIENTED_EDGE('',*,*,#5588,.F.);
#7585=ORIENTED_EDGE('',*,*,#5610,.F.);
#7586=ORIENTED_EDGE('',*,*,#5613,.F.);
#7587=ORIENTED_EDGE('',*,*,#5612,.T.);
#7588=ORIENTED_EDGE('',*,*,#5614,.T.);
#7589=ORIENTED_EDGE('',*,*,#5615,.T.);
#7590=ORIENTED_EDGE('',*,*,#5592,.T.);
#7591=ORIENTED_EDGE('',*,*,#5616,.F.);
#7592=ORIENTED_EDGE('',*,*,#5617,.F.);
#7593=ORIENTED_EDGE('',*,*,#5593,.F.);
#7594=ORIENTED_EDGE('',*,*,#5615,.F.);
#7595=ORIENTED_EDGE('',*,*,#5617,.T.);
#7596=ORIENTED_EDGE('',*,*,#5618,.T.);
#7597=ORIENTED_EDGE('',*,*,#5619,.T.);
#7598=ORIENTED_EDGE('',*,*,#5594,.T.);
#7599=ORIENTED_EDGE('',*,*,#5620,.F.);
#7600=ORIENTED_EDGE('',*,*,#5621,.F.);
#7601=ORIENTED_EDGE('',*,*,#5595,.F.);
#7602=ORIENTED_EDGE('',*,*,#5619,.F.);
#7603=ORIENTED_EDGE('',*,*,#5621,.T.);
#7604=ORIENTED_EDGE('',*,*,#5622,.T.);
#7605=ORIENTED_EDGE('',*,*,#5623,.T.);
#7606=ORIENTED_EDGE('',*,*,#5596,.T.);
#7607=ORIENTED_EDGE('',*,*,#5597,.F.);
#7608=ORIENTED_EDGE('',*,*,#5623,.F.);
#7609=ORIENTED_EDGE('',*,*,#5624,.F.);
#7610=ORIENTED_EDGE('',*,*,#5625,.F.);
#7611=ORIENTED_EDGE('',*,*,#5626,.F.);
#7612=ORIENTED_EDGE('',*,*,#5627,.T.);
#7613=ORIENTED_EDGE('',*,*,#5613,.T.);
#7614=ORIENTED_EDGE('',*,*,#5609,.F.);
#7615=ORIENTED_EDGE('',*,*,#5607,.T.);
#7616=ORIENTED_EDGE('',*,*,#5605,.F.);
#7617=ORIENTED_EDGE('',*,*,#5603,.T.);
#7618=ORIENTED_EDGE('',*,*,#5601,.F.);
#7619=ORIENTED_EDGE('',*,*,#5579,.T.);
#7620=ORIENTED_EDGE('',*,*,#5628,.F.);
#7621=ORIENTED_EDGE('',*,*,#5629,.T.);
#7622=ORIENTED_EDGE('',*,*,#5630,.F.);
#7623=ORIENTED_EDGE('',*,*,#5624,.T.);
#7624=ORIENTED_EDGE('',*,*,#5622,.F.);
#7625=ORIENTED_EDGE('',*,*,#5620,.T.);
#7626=ORIENTED_EDGE('',*,*,#5618,.F.);
#7627=ORIENTED_EDGE('',*,*,#5616,.T.);
#7628=ORIENTED_EDGE('',*,*,#5614,.F.);
#7629=ORIENTED_EDGE('',*,*,#5611,.T.);
#7630=ORIENTED_EDGE('',*,*,#5627,.F.);
#7631=ORIENTED_EDGE('',*,*,#5582,.T.);
#7632=ORIENTED_EDGE('',*,*,#5600,.T.);
#7633=ORIENTED_EDGE('',*,*,#5631,.T.);
#7634=ORIENTED_EDGE('',*,*,#5628,.T.);
#7635=ORIENTED_EDGE('',*,*,#5599,.F.);
#7636=ORIENTED_EDGE('',*,*,#5632,.F.);
#7637=ORIENTED_EDGE('',*,*,#5629,.F.);
#7638=ORIENTED_EDGE('',*,*,#5631,.F.);
#7639=ORIENTED_EDGE('',*,*,#5590,.T.);
#7640=ORIENTED_EDGE('',*,*,#5626,.T.);
#7641=ORIENTED_EDGE('',*,*,#5625,.T.);
#7642=ORIENTED_EDGE('',*,*,#5630,.T.);
#7643=ORIENTED_EDGE('',*,*,#5632,.T.);
#7644=ORIENTED_EDGE('',*,*,#5598,.T.);
#7645=ORIENTED_EDGE('',*,*,#5633,.F.);
#7646=ORIENTED_EDGE('',*,*,#5634,.T.);
#7647=ORIENTED_EDGE('',*,*,#5635,.F.);
#7648=ORIENTED_EDGE('',*,*,#5636,.T.);
#7649=ORIENTED_EDGE('',*,*,#5633,.T.);
#7650=ORIENTED_EDGE('',*,*,#5636,.F.);
#7651=ORIENTED_EDGE('',*,*,#5635,.T.);
#7652=ORIENTED_EDGE('',*,*,#5637,.F.);
#7653=ORIENTED_EDGE('',*,*,#5637,.T.);
#7654=ORIENTED_EDGE('',*,*,#5638,.T.);
#7655=ORIENTED_EDGE('',*,*,#5634,.F.);
#7656=ORIENTED_EDGE('',*,*,#5638,.F.);
#7657=ORIENTED_EDGE('',*,*,#5639,.F.);
#7658=ORIENTED_EDGE('',*,*,#5640,.T.);
#7659=ORIENTED_EDGE('',*,*,#5641,.F.);
#7660=ORIENTED_EDGE('',*,*,#5642,.T.);
#7661=ORIENTED_EDGE('',*,*,#5639,.T.);
#7662=ORIENTED_EDGE('',*,*,#5642,.F.);
#7663=ORIENTED_EDGE('',*,*,#5641,.T.);
#7664=ORIENTED_EDGE('',*,*,#5643,.F.);
#7665=ORIENTED_EDGE('',*,*,#5643,.T.);
#7666=ORIENTED_EDGE('',*,*,#5644,.T.);
#7667=ORIENTED_EDGE('',*,*,#5640,.F.);
#7668=ORIENTED_EDGE('',*,*,#5644,.F.);
#7669=CYLINDRICAL_SURFACE('',#9043,0.210000000000001);
#7670=CYLINDRICAL_SURFACE('',#9046,0.210000000000001);
#7671=CYLINDRICAL_SURFACE('',#9049,0.210000000000001);
#7672=CYLINDRICAL_SURFACE('',#9052,0.210000000000001);
#7673=CYLINDRICAL_SURFACE('',#9055,0.21);
#7674=CYLINDRICAL_SURFACE('',#9058,0.21);
#7675=CYLINDRICAL_SURFACE('',#9061,0.21);
#7676=CYLINDRICAL_SURFACE('',#9064,0.21);
#7677=CYLINDRICAL_SURFACE('',#9067,0.210000000000001);
#7678=CYLINDRICAL_SURFACE('',#9070,0.210000000000001);
#7679=CYLINDRICAL_SURFACE('',#9073,0.210000000000001);
#7680=CYLINDRICAL_SURFACE('',#9076,0.210000000000001);
#7681=CYLINDRICAL_SURFACE('',#9079,0.21);
#7682=CYLINDRICAL_SURFACE('',#9082,0.21);
#7683=CYLINDRICAL_SURFACE('',#9085,0.21);
#7684=CYLINDRICAL_SURFACE('',#9088,0.21);
#7685=CYLINDRICAL_SURFACE('',#9091,0.25);
#7686=CYLINDRICAL_SURFACE('',#9094,0.25);
#7687=CYLINDRICAL_SURFACE('',#9097,0.25);
#7688=CYLINDRICAL_SURFACE('',#9100,0.25);
#7689=CYLINDRICAL_SURFACE('',#9110,0.6);
#7690=CYLINDRICAL_SURFACE('',#9113,0.6);
#7691=CYLINDRICAL_SURFACE('',#9116,0.6);
#7692=CYLINDRICAL_SURFACE('',#9119,0.6);
#7693=CYLINDRICAL_SURFACE('',#9122,0.165);
#7694=CYLINDRICAL_SURFACE('',#9126,0.165);
#7695=CYLINDRICAL_SURFACE('',#9130,0.165);
#7696=CYLINDRICAL_SURFACE('',#9134,0.165);
#7697=CYLINDRICAL_SURFACE('',#9138,0.6);
#7698=CYLINDRICAL_SURFACE('',#9143,0.6);
#7699=CYLINDRICAL_SURFACE('',#9148,0.6);
#7700=CYLINDRICAL_SURFACE('',#9153,0.6);
#7701=CYLINDRICAL_SURFACE('',#9164,0.33);
#7702=CYLINDRICAL_SURFACE('',#9166,0.33);
#7703=CYLINDRICAL_SURFACE('',#9168,0.33);
#7704=CYLINDRICAL_SURFACE('',#9170,0.33);
#7705=CYLINDRICAL_SURFACE('',#9172,2.6);
#7706=CYLINDRICAL_SURFACE('',#9174,2.2);
#7707=CYLINDRICAL_SURFACE('',#9177,4.);
#7708=CYLINDRICAL_SURFACE('',#9182,0.225);
#7709=CYLINDRICAL_SURFACE('',#9185,0.225);
#7710=CYLINDRICAL_SURFACE('',#9188,0.225);
#7711=CYLINDRICAL_SURFACE('',#9191,0.225);
#7712=CYLINDRICAL_SURFACE('',#9194,2.59);
#7713=CYLINDRICAL_SURFACE('',#9199,2.);
#7714=CYLINDRICAL_SURFACE('',#9201,4.);
#7715=CYLINDRICAL_SURFACE('',#9221,0.5);
#7716=CYLINDRICAL_SURFACE('',#9229,0.2942);
#7717=CYLINDRICAL_SURFACE('',#9238,1.88531);
#7718=CYLINDRICAL_SURFACE('',#9240,1.25);
#7719=CYLINDRICAL_SURFACE('',#9246,1.88531);
#7720=CYLINDRICAL_SURFACE('',#9258,1.96469);
#7721=CYLINDRICAL_SURFACE('',#9265,2.6);
#7722=CYLINDRICAL_SURFACE('',#9270,1.96469);
#7723=CYLINDRICAL_SURFACE('',#9294,1.956752);
#7724=CYLINDRICAL_SURFACE('',#9342,1.893248);
#7725=CYLINDRICAL_SURFACE('',#9356,1.95469);
#7726=CYLINDRICAL_SURFACE('',#9360,1.90031);
#7727=CYLINDRICAL_SURFACE('',#9364,1.95469);
#7728=CYLINDRICAL_SURFACE('',#9368,1.90031);
#7729=CYLINDRICAL_SURFACE('',#9390,0.165);
#7730=CYLINDRICAL_SURFACE('',#9394,0.165);
#7731=CYLINDRICAL_SURFACE('',#9398,0.165);
#7732=CYLINDRICAL_SURFACE('',#9405,1.75);
#7733=CYLINDRICAL_SURFACE('',#9407,1.25);
#7734=CYLINDRICAL_SURFACE('',#9412,0.225);
#7735=CYLINDRICAL_SURFACE('',#9415,0.225);
#7736=CYLINDRICAL_SURFACE('',#9418,0.225);
#7737=CYLINDRICAL_SURFACE('',#9421,0.25);
#7738=CYLINDRICAL_SURFACE('',#9424,0.25);
#7739=CYLINDRICAL_SURFACE('',#9427,0.25);
#7740=CYLINDRICAL_SURFACE('',#9430,0.25);
#7741=CYLINDRICAL_SURFACE('',#9433,0.25);
#7742=CYLINDRICAL_SURFACE('',#9436,0.25);
#7743=CYLINDRICAL_SURFACE('',#9439,0.25);
#7744=CYLINDRICAL_SURFACE('',#9442,0.25);
#7745=CYLINDRICAL_SURFACE('',#9445,0.25);
#7746=CYLINDRICAL_SURFACE('',#9448,20.);
#7747=CYLINDRICAL_SURFACE('',#9457,0.21);
#7748=CYLINDRICAL_SURFACE('',#9460,1.255);
#7749=CYLINDRICAL_SURFACE('',#9463,1.8);
#7750=CYLINDRICAL_SURFACE('',#9473,0.35);
#7751=CYLINDRICAL_SURFACE('',#9481,0.1954);
#7752=CYLINDRICAL_SURFACE('',#9520,0.24505);
#7753=CYLINDRICAL_SURFACE('',#9534,0.275);
#7754=CYLINDRICAL_SURFACE('',#9537,0.275);
#7755=CYLINDRICAL_SURFACE('',#9540,0.275);
#7756=CYLINDRICAL_SURFACE('',#9543,0.275);
#7757=CYLINDRICAL_SURFACE('',#9546,0.5);
#7758=CYLINDRICAL_SURFACE('',#9549,0.5);
#7759=CYLINDRICAL_SURFACE('',#9569,0.165);
#7760=CYLINDRICAL_SURFACE('',#9576,0.8);
#7761=CYLINDRICAL_SURFACE('',#9579,0.5);
#7762=CYLINDRICAL_SURFACE('',#9583,0.505);
#7763=CYLINDRICAL_SURFACE('',#9586,0.7);
#7764=CYLINDRICAL_SURFACE('',#9592,0.505);
#7765=CYLINDRICAL_SURFACE('',#9595,0.7);
#7766=CYLINDRICAL_SURFACE('',#9601,0.225);
#7767=CYLINDRICAL_SURFACE('',#9604,0.8);
#7768=CYLINDRICAL_SURFACE('',#9611,0.275);
#7769=CYLINDRICAL_SURFACE('',#9614,0.275);
#7770=CYLINDRICAL_SURFACE('',#9617,0.275);
#7771=CYLINDRICAL_SURFACE('',#9620,0.275);
#7772=CYLINDRICAL_SURFACE('',#9623,0.5);
#7773=CYLINDRICAL_SURFACE('',#9626,0.5);
#7774=CYLINDRICAL_SURFACE('',#9646,0.165);
#7775=CYLINDRICAL_SURFACE('',#9653,0.8);
#7776=CYLINDRICAL_SURFACE('',#9656,0.5);
#7777=CYLINDRICAL_SURFACE('',#9660,0.505);
#7778=CYLINDRICAL_SURFACE('',#9663,0.7);
#7779=CYLINDRICAL_SURFACE('',#9669,0.505);
#7780=CYLINDRICAL_SURFACE('',#9672,0.7);
#7781=CYLINDRICAL_SURFACE('',#9678,0.225);
#7782=CYLINDRICAL_SURFACE('',#9681,0.8);
#7783=CYLINDRICAL_SURFACE('',#9688,0.275);
#7784=CYLINDRICAL_SURFACE('',#9691,0.275);
#7785=CYLINDRICAL_SURFACE('',#9694,0.275);
#7786=CYLINDRICAL_SURFACE('',#9697,0.275);
#7787=CYLINDRICAL_SURFACE('',#9700,0.5);
#7788=CYLINDRICAL_SURFACE('',#9703,0.5);
#7789=CYLINDRICAL_SURFACE('',#9723,0.165);
#7790=CYLINDRICAL_SURFACE('',#9730,0.8);
#7791=CYLINDRICAL_SURFACE('',#9733,0.5);
#7792=CYLINDRICAL_SURFACE('',#9737,0.505);
#7793=CYLINDRICAL_SURFACE('',#9740,0.7);
#7794=CYLINDRICAL_SURFACE('',#9746,0.505);
#7795=CYLINDRICAL_SURFACE('',#9749,0.7);
#7796=CYLINDRICAL_SURFACE('',#9755,0.225);
#7797=CYLINDRICAL_SURFACE('',#9758,0.8);
#7798=CYLINDRICAL_SURFACE('',#9765,0.275);
#7799=CYLINDRICAL_SURFACE('',#9768,0.275);
#7800=CYLINDRICAL_SURFACE('',#9771,0.275);
#7801=CYLINDRICAL_SURFACE('',#9774,0.275);
#7802=CYLINDRICAL_SURFACE('',#9777,0.5);
#7803=CYLINDRICAL_SURFACE('',#9780,0.5);
#7804=CYLINDRICAL_SURFACE('',#9800,0.165);
#7805=CYLINDRICAL_SURFACE('',#9807,0.8);
#7806=CYLINDRICAL_SURFACE('',#9810,0.5);
#7807=CYLINDRICAL_SURFACE('',#9814,0.505);
#7808=CYLINDRICAL_SURFACE('',#9817,0.7);
#7809=CYLINDRICAL_SURFACE('',#9823,0.505);
#7810=CYLINDRICAL_SURFACE('',#9826,0.7);
#7811=CYLINDRICAL_SURFACE('',#9832,0.225);
#7812=CYLINDRICAL_SURFACE('',#9835,0.8);
#7813=CYLINDRICAL_SURFACE('',#9855,0.425);
#7814=CYLINDRICAL_SURFACE('',#9863,0.24505);
#7815=CYLINDRICAL_SURFACE('',#9879,0.35);
#7816=CYLINDRICAL_SURFACE('',#9887,0.1954);
#7817=CYLINDRICAL_SURFACE('',#9930,1.5);
#7818=CYLINDRICAL_SURFACE('',#9933,2.);
#7819=CYLINDRICAL_SURFACE('',#9939,1.1);
#7820=CYLINDRICAL_SURFACE('',#9942,1.5);
#7821=CYLINDRICAL_SURFACE('',#9948,1.1);
#7822=CYLINDRICAL_SURFACE('',#9951,1.5);
#7823=CYLINDRICAL_SURFACE('',#9958,1.5);
#7824=CYLINDRICAL_SURFACE('',#9961,2.);
#7825=CYLINDRICAL_SURFACE('',#9967,1.1);
#7826=CYLINDRICAL_SURFACE('',#9970,1.5);
#7827=CYLINDRICAL_SURFACE('',#9976,1.1);
#7828=CYLINDRICAL_SURFACE('',#9979,1.5);
#7829=CYLINDRICAL_SURFACE('',#9986,1.5);
#7830=CYLINDRICAL_SURFACE('',#9989,2.);
#7831=CYLINDRICAL_SURFACE('',#9995,1.1);
#7832=CYLINDRICAL_SURFACE('',#9998,1.5);
#7833=CYLINDRICAL_SURFACE('',#10004,1.1);
#7834=CYLINDRICAL_SURFACE('',#10007,1.5);
#7835=CYLINDRICAL_SURFACE('',#10014,1.5);
#7836=CYLINDRICAL_SURFACE('',#10017,2.);
#7837=CYLINDRICAL_SURFACE('',#10023,1.1);
#7838=CYLINDRICAL_SURFACE('',#10026,1.5);
#7839=CYLINDRICAL_SURFACE('',#10032,1.1);
#7840=CYLINDRICAL_SURFACE('',#10035,1.5);
#7841=CYLINDRICAL_SURFACE('',#10048,0.976185);
#7842=CYLINDRICAL_SURFACE('',#10050,0.5);
#7843=CYLINDRICAL_SURFACE('',#10056,0.976185);
#7844=CYLINDRICAL_SURFACE('',#10068,1.023815);
#7845=CYLINDRICAL_SURFACE('',#10075,1.5);
#7846=CYLINDRICAL_SURFACE('',#10080,1.023815);
#7847=CYLINDRICAL_SURFACE('',#10102,1.019052);
#7848=CYLINDRICAL_SURFACE('',#10142,0.980948);
#7849=CYLINDRICAL_SURFACE('',#10156,1.013815);
#7850=CYLINDRICAL_SURFACE('',#10160,0.991185);
#7851=CYLINDRICAL_SURFACE('',#10164,1.013815);
#7852=CYLINDRICAL_SURFACE('',#10168,0.991185);
#7853=ADVANCED_FACE('',(#1250),#7669,.F.);
#7854=ADVANCED_FACE('',(#1251),#7670,.F.);
#7855=ADVANCED_FACE('',(#1252),#7671,.F.);
#7856=ADVANCED_FACE('',(#1253),#7672,.F.);
#7857=ADVANCED_FACE('',(#1254),#7673,.F.);
#7858=ADVANCED_FACE('',(#1255),#7674,.F.);
#7859=ADVANCED_FACE('',(#1256),#7675,.F.);
#7860=ADVANCED_FACE('',(#1257),#7676,.F.);
#7861=ADVANCED_FACE('',(#1258),#7677,.F.);
#7862=ADVANCED_FACE('',(#1259),#7678,.F.);
#7863=ADVANCED_FACE('',(#1260),#7679,.F.);
#7864=ADVANCED_FACE('',(#1261),#7680,.F.);
#7865=ADVANCED_FACE('',(#1262),#7681,.F.);
#7866=ADVANCED_FACE('',(#1263),#7682,.F.);
#7867=ADVANCED_FACE('',(#1264),#7683,.F.);
#7868=ADVANCED_FACE('',(#1265),#7684,.F.);
#7869=ADVANCED_FACE('',(#1266),#7685,.F.);
#7870=ADVANCED_FACE('',(#1267),#7686,.F.);
#7871=ADVANCED_FACE('',(#1268),#7687,.F.);
#7872=ADVANCED_FACE('',(#1269),#7688,.F.);
#7873=ADVANCED_FACE('',(#1270),#990,.T.);
#7874=ADVANCED_FACE('',(#1271),#991,.T.);
#7875=ADVANCED_FACE('',(#1272),#992,.T.);
#7876=ADVANCED_FACE('',(#1273),#993,.T.);
#7877=ADVANCED_FACE('',(#1274,#757,#758,#759,#760,#761,#762,#763,#764,#765,
#766,#767,#768,#769,#770,#771,#772,#773,#774,#775,#776),#994,.T.);
#7878=ADVANCED_FACE('',(#1275,#777,#778,#779,#780,#781,#782,#783,#784,#785,
#786,#787,#788,#789,#790,#791,#792,#793,#794,#795,#796),#995,.F.);
#7879=ADVANCED_FACE('',(#1276),#7689,.F.);
#7880=ADVANCED_FACE('',(#1277),#7690,.F.);
#7881=ADVANCED_FACE('',(#1278),#7691,.F.);
#7882=ADVANCED_FACE('',(#1279),#7692,.F.);
#7883=ADVANCED_FACE('',(#1280),#7693,.F.);
#7884=ADVANCED_FACE('',(#1281),#996,.T.);
#7885=ADVANCED_FACE('',(#1282),#7694,.F.);
#7886=ADVANCED_FACE('',(#1283),#997,.T.);
#7887=ADVANCED_FACE('',(#1284),#7695,.F.);
#7888=ADVANCED_FACE('',(#1285),#998,.T.);
#7889=ADVANCED_FACE('',(#1286),#7696,.F.);
#7890=ADVANCED_FACE('',(#1287),#999,.T.);
#7891=ADVANCED_FACE('',(#1288),#7697,.F.);
#7892=ADVANCED_FACE('',(#1289,#797),#1000,.T.);
#7893=ADVANCED_FACE('',(#1290),#7698,.F.);
#7894=ADVANCED_FACE('',(#1291,#798),#1001,.T.);
#7895=ADVANCED_FACE('',(#1292),#7699,.F.);
#7896=ADVANCED_FACE('',(#1293,#799),#1002,.T.);
#7897=ADVANCED_FACE('',(#1294),#7700,.F.);
#7898=ADVANCED_FACE('',(#1295,#800),#1003,.T.);
#7899=ADVANCED_FACE('',(#1296,#801,#802,#803,#804,#805),#1004,.T.);
#7900=ADVANCED_FACE('',(#1297),#7701,.F.);
#7901=ADVANCED_FACE('',(#1298),#7702,.F.);
#7902=ADVANCED_FACE('',(#1299),#7703,.F.);
#7903=ADVANCED_FACE('',(#1300),#7704,.F.);
#7904=ADVANCED_FACE('',(#1301),#7705,.F.);
#7905=ADVANCED_FACE('',(#1302),#7706,.F.);
#7906=ADVANCED_FACE('',(#1303),#7707,.T.);
#7907=ADVANCED_FACE('',(#1304,#806),#1005,.T.);
#7908=ADVANCED_FACE('',(#1305,#807,#808,#809,#810,#811),#1006,.F.);
#7909=ADVANCED_FACE('',(#1306),#7708,.F.);
#7910=ADVANCED_FACE('',(#1307),#7709,.F.);
#7911=ADVANCED_FACE('',(#1308),#7710,.F.);
#7912=ADVANCED_FACE('',(#1309),#7711,.F.);
#7913=ADVANCED_FACE('',(#1310),#7712,.T.);
#7914=ADVANCED_FACE('',(#1311,#812),#1007,.F.);
#7915=ADVANCED_FACE('',(#1312),#7713,.F.);
#7916=ADVANCED_FACE('',(#1313),#7714,.T.);
#7917=ADVANCED_FACE('',(#1314,#813,#814,#815,#816,#817),#1008,.T.);
#7918=ADVANCED_FACE('',(#1315,#818,#819,#820,#821,#822),#1009,.F.);
#7919=ADVANCED_FACE('',(#1316),#1010,.F.);
#7920=ADVANCED_FACE('',(#1317),#1011,.F.);
#7921=ADVANCED_FACE('',(#1318),#1012,.F.);
#7922=ADVANCED_FACE('',(#1319),#1013,.F.);
#7923=ADVANCED_FACE('',(#1320),#1014,.F.);
#7924=ADVANCED_FACE('',(#1321),#1015,.F.);
#7925=ADVANCED_FACE('',(#1322),#1016,.F.);
#7926=ADVANCED_FACE('',(#1323),#1017,.F.);
#7927=ADVANCED_FACE('',(#1324),#1018,.F.);
#7928=ADVANCED_FACE('',(#1325),#1019,.T.);
#7929=ADVANCED_FACE('',(#1326),#476,.T.);
#7930=ADVANCED_FACE('',(#1327),#7715,.T.);
#7931=ADVANCED_FACE('',(#1328),#477,.T.);
#7932=ADVANCED_FACE('',(#1329,#823),#1020,.T.);
#7933=ADVANCED_FACE('',(#1330),#478,.T.);
#7934=ADVANCED_FACE('',(#1331),#7716,.T.);
#7935=ADVANCED_FACE('',(#1332),#472,.F.);
#7936=ADVANCED_FACE('',(#1333),#7717,.T.);
#7937=ADVANCED_FACE('',(#1334),#7718,.F.);
#7938=ADVANCED_FACE('',(#1335),#479,.F.);
#7939=ADVANCED_FACE('',(#1336,#824),#1021,.T.);
#7940=ADVANCED_FACE('',(#1337),#7719,.T.);
#7941=ADVANCED_FACE('',(#1338,#825),#1022,.T.);
#7942=ADVANCED_FACE('',(#1339),#480,.F.);
#7943=ADVANCED_FACE('',(#1340),#473,.F.);
#7944=ADVANCED_FACE('',(#1341),#7720,.F.);
#7945=ADVANCED_FACE('',(#1342,#826),#1023,.T.);
#7946=ADVANCED_FACE('',(#1343),#481,.T.);
#7947=ADVANCED_FACE('',(#1344),#7721,.T.);
#7948=ADVANCED_FACE('',(#1345),#482,.T.);
#7949=ADVANCED_FACE('',(#1346,#827),#1024,.T.);
#7950=ADVANCED_FACE('',(#1347),#7722,.F.);
#7951=ADVANCED_FACE('',(#1348),#438,.T.);
#7952=ADVANCED_FACE('',(#1349),#439,.T.);
#7953=ADVANCED_FACE('',(#1350),#440,.T.);
#7954=ADVANCED_FACE('',(#1351),#441,.T.);
#7955=ADVANCED_FACE('',(#1352),#442,.T.);
#7956=ADVANCED_FACE('',(#1353),#443,.T.);
#7957=ADVANCED_FACE('',(#1354),#444,.T.);
#7958=ADVANCED_FACE('',(#1355),#445,.T.);
#7959=ADVANCED_FACE('',(#1356),#446,.T.);
#7960=ADVANCED_FACE('',(#1357),#447,.F.);
#7961=ADVANCED_FACE('',(#1358),#7723,.T.);
#7962=ADVANCED_FACE('',(#1359),#1025,.T.);
#7963=ADVANCED_FACE('',(#1360),#448,.F.);
#7964=ADVANCED_FACE('',(#1361),#1026,.T.);
#7965=ADVANCED_FACE('',(#1362),#449,.F.);
#7966=ADVANCED_FACE('',(#1363),#1027,.T.);
#7967=ADVANCED_FACE('',(#1364),#450,.F.);
#7968=ADVANCED_FACE('',(#1365),#1028,.T.);
#7969=ADVANCED_FACE('',(#1366),#451,.F.);
#7970=ADVANCED_FACE('',(#1367),#1029,.T.);
#7971=ADVANCED_FACE('',(#1368),#452,.F.);
#7972=ADVANCED_FACE('',(#1369),#1030,.T.);
#7973=ADVANCED_FACE('',(#1370),#453,.F.);
#7974=ADVANCED_FACE('',(#1371),#1031,.T.);
#7975=ADVANCED_FACE('',(#1372),#454,.F.);
#7976=ADVANCED_FACE('',(#1373),#7724,.F.);
#7977=ADVANCED_FACE('',(#1374),#1032,.T.);
#7978=ADVANCED_FACE('',(#1375),#455,.F.);
#7979=ADVANCED_FACE('',(#1376,#828),#1033,.T.);
#7980=ADVANCED_FACE('',(#1377),#1034,.T.);
#7981=ADVANCED_FACE('',(#1378,#829),#1035,.T.);
#7982=ADVANCED_FACE('',(#1379),#7725,.T.);
#7983=ADVANCED_FACE('',(#1380,#830),#1036,.T.);
#7984=ADVANCED_FACE('',(#1381),#7726,.F.);
#7985=ADVANCED_FACE('',(#1382,#831),#1037,.T.);
#7986=ADVANCED_FACE('',(#1383),#7727,.T.);
#7987=ADVANCED_FACE('',(#1384,#832),#1038,.T.);
#7988=ADVANCED_FACE('',(#1385),#7728,.F.);
#7989=ADVANCED_FACE('',(#1386),#1039,.T.);
#7990=ADVANCED_FACE('',(#1387),#1040,.T.);
#7991=ADVANCED_FACE('',(#1388),#1041,.T.);
#7992=ADVANCED_FACE('',(#1389),#1042,.T.);
#7993=ADVANCED_FACE('',(#1390),#1043,.T.);
#7994=ADVANCED_FACE('',(#1391),#1044,.F.);
#7995=ADVANCED_FACE('',(#1392),#1045,.T.);
#7996=ADVANCED_FACE('',(#1393),#1046,.T.);
#7997=ADVANCED_FACE('',(#1394),#1047,.T.);
#7998=ADVANCED_FACE('',(#1395),#1048,.T.);
#7999=ADVANCED_FACE('',(#1396),#1049,.T.);
#8000=ADVANCED_FACE('',(#1397),#1050,.F.);
#8001=ADVANCED_FACE('',(#1398),#7729,.F.);
#8002=ADVANCED_FACE('',(#1399),#1051,.T.);
#8003=ADVANCED_FACE('',(#1400),#7730,.F.);
#8004=ADVANCED_FACE('',(#1401),#1052,.T.);
#8005=ADVANCED_FACE('',(#1402),#7731,.F.);
#8006=ADVANCED_FACE('',(#1403),#1053,.T.);
#8007=ADVANCED_FACE('',(#1404,#833),#1054,.F.);
#8008=ADVANCED_FACE('',(#1405),#7732,.T.);
#8009=ADVANCED_FACE('',(#1406),#7733,.T.);
#8010=ADVANCED_FACE('',(#1407,#834,#835,#836),#1055,.T.);
#8011=ADVANCED_FACE('',(#1408),#1056,.F.);
#8012=ADVANCED_FACE('',(#1409),#7734,.F.);
#8013=ADVANCED_FACE('',(#1410),#7735,.F.);
#8014=ADVANCED_FACE('',(#1411),#7736,.F.);
#8015=ADVANCED_FACE('',(#1412),#7737,.F.);
#8016=ADVANCED_FACE('',(#1413),#7738,.F.);
#8017=ADVANCED_FACE('',(#1414),#7739,.F.);
#8018=ADVANCED_FACE('',(#1415),#7740,.F.);
#8019=ADVANCED_FACE('',(#1416),#7741,.F.);
#8020=ADVANCED_FACE('',(#1417),#7742,.F.);
#8021=ADVANCED_FACE('',(#1418),#7743,.F.);
#8022=ADVANCED_FACE('',(#1419),#7744,.F.);
#8023=ADVANCED_FACE('',(#1420),#7745,.F.);
#8024=ADVANCED_FACE('',(#1421),#7746,.T.);
#8025=ADVANCED_FACE('',(#1422,#837,#838,#839,#840,#841,#842,#843,#844,#845,
#846,#847,#848),#1057,.T.);
#8026=ADVANCED_FACE('',(#1423,#849,#850,#851,#852,#853,#854,#855,#856,#857,
#858,#859,#860),#1058,.F.);
#8027=ADVANCED_FACE('',(#1424),#1059,.T.);
#8028=ADVANCED_FACE('',(#1425),#7747,.F.);
#8029=ADVANCED_FACE('',(#1426),#1060,.T.);
#8030=ADVANCED_FACE('',(#1427,#861),#7748,.F.);
#8031=ADVANCED_FACE('',(#1428,#862),#7749,.T.);
#8032=ADVANCED_FACE('',(#1429,#863),#1061,.T.);
#8033=ADVANCED_FACE('',(#1430,#864),#1062,.F.);
#8034=ADVANCED_FACE('',(#1431),#1063,.T.);
#8035=ADVANCED_FACE('',(#1432),#483,.T.);
#8036=ADVANCED_FACE('',(#1433),#7750,.T.);
#8037=ADVANCED_FACE('',(#1434),#484,.T.);
#8038=ADVANCED_FACE('',(#1435,#865),#1064,.T.);
#8039=ADVANCED_FACE('',(#1436),#485,.T.);
#8040=ADVANCED_FACE('',(#1437),#7751,.T.);
#8041=ADVANCED_FACE('',(#1438),#486,.T.);
#8042=ADVANCED_FACE('',(#1439),#1065,.T.);
#8043=ADVANCED_FACE('',(#1440),#1066,.F.);
#8044=ADVANCED_FACE('',(#1441),#1067,.F.);
#8045=ADVANCED_FACE('',(#1442),#1068,.F.);
#8046=ADVANCED_FACE('',(#1443),#1069,.F.);
#8047=ADVANCED_FACE('',(#1444),#1070,.F.);
#8048=ADVANCED_FACE('',(#1445),#1071,.F.);
#8049=ADVANCED_FACE('',(#1446),#1072,.F.);
#8050=ADVANCED_FACE('',(#1447),#1073,.F.);
#8051=ADVANCED_FACE('',(#1448),#1074,.F.);
#8052=ADVANCED_FACE('',(#1449),#1075,.F.);
#8053=ADVANCED_FACE('',(#1450),#1076,.F.);
#8054=ADVANCED_FACE('',(#1451),#1077,.F.);
#8055=ADVANCED_FACE('',(#1452),#1078,.F.);
#8056=ADVANCED_FACE('',(#1453),#1079,.F.);
#8057=ADVANCED_FACE('',(#1454),#1080,.F.);
#8058=ADVANCED_FACE('',(#1455,#866),#1081,.T.);
#8059=ADVANCED_FACE('',(#1456),#487,.T.);
#8060=ADVANCED_FACE('',(#1457),#7752,.T.);
#8061=ADVANCED_FACE('',(#1458),#488,.T.);
#8062=ADVANCED_FACE('',(#1459),#1082,.T.);
#8063=ADVANCED_FACE('',(#1460),#7753,.F.);
#8064=ADVANCED_FACE('',(#1461),#7754,.F.);
#8065=ADVANCED_FACE('',(#1462),#7755,.F.);
#8066=ADVANCED_FACE('',(#1463),#7756,.F.);
#8067=ADVANCED_FACE('',(#1464),#7757,.F.);
#8068=ADVANCED_FACE('',(#1465),#7758,.F.);
#8069=ADVANCED_FACE('',(#1466),#1083,.T.);
#8070=ADVANCED_FACE('',(#1467),#1084,.T.);
#8071=ADVANCED_FACE('',(#1468),#1085,.T.);
#8072=ADVANCED_FACE('',(#1469,#867),#1086,.T.);
#8073=ADVANCED_FACE('',(#1470,#868),#1087,.F.);
#8074=ADVANCED_FACE('',(#1471),#1088,.T.);
#8075=ADVANCED_FACE('',(#1472),#1089,.T.);
#8076=ADVANCED_FACE('',(#1473),#1090,.T.);
#8077=ADVANCED_FACE('',(#1474,#869),#1091,.T.);
#8078=ADVANCED_FACE('',(#1475,#870),#1092,.F.);
#8079=ADVANCED_FACE('',(#1476),#1093,.T.);
#8080=ADVANCED_FACE('',(#1477),#1094,.T.);
#8081=ADVANCED_FACE('',(#1478),#1095,.T.);
#8082=ADVANCED_FACE('',(#1479),#1096,.T.);
#8083=ADVANCED_FACE('',(#1480,#871,#872,#873,#874,#875,#876),#1097,.T.);
#8084=ADVANCED_FACE('',(#1481,#877,#878,#879,#880),#1098,.F.);
#8085=ADVANCED_FACE('',(#1482),#7759,.F.);
#8086=ADVANCED_FACE('',(#1483),#1099,.T.);
#8087=ADVANCED_FACE('',(#1484,#881),#1100,.T.);
#8088=ADVANCED_FACE('',(#1485),#7760,.T.);
#8089=ADVANCED_FACE('',(#1486),#1101,.F.);
#8090=ADVANCED_FACE('',(#1487),#7761,.T.);
#8091=ADVANCED_FACE('',(#1488,#882),#1102,.T.);
#8092=ADVANCED_FACE('',(#1489),#7762,.F.);
#8093=ADVANCED_FACE('',(#1490),#7763,.T.);
#8094=ADVANCED_FACE('',(#1491,#883),#1103,.T.);
#8095=ADVANCED_FACE('',(#1492,#884),#1104,.F.);
#8096=ADVANCED_FACE('',(#1493),#7764,.F.);
#8097=ADVANCED_FACE('',(#1494),#7765,.T.);
#8098=ADVANCED_FACE('',(#1495,#885),#1105,.T.);
#8099=ADVANCED_FACE('',(#1496,#886),#1106,.F.);
#8100=ADVANCED_FACE('',(#1497),#7766,.F.);
#8101=ADVANCED_FACE('',(#1498),#7767,.T.);
#8102=ADVANCED_FACE('',(#1499,#887),#1107,.T.);
#8103=ADVANCED_FACE('',(#1500,#888),#1108,.F.);
#8104=ADVANCED_FACE('',(#1501),#7768,.F.);
#8105=ADVANCED_FACE('',(#1502),#7769,.F.);
#8106=ADVANCED_FACE('',(#1503),#7770,.F.);
#8107=ADVANCED_FACE('',(#1504),#7771,.F.);
#8108=ADVANCED_FACE('',(#1505),#7772,.F.);
#8109=ADVANCED_FACE('',(#1506),#7773,.F.);
#8110=ADVANCED_FACE('',(#1507),#1109,.T.);
#8111=ADVANCED_FACE('',(#1508),#1110,.T.);
#8112=ADVANCED_FACE('',(#1509),#1111,.T.);
#8113=ADVANCED_FACE('',(#1510,#889),#1112,.T.);
#8114=ADVANCED_FACE('',(#1511,#890),#1113,.F.);
#8115=ADVANCED_FACE('',(#1512),#1114,.T.);
#8116=ADVANCED_FACE('',(#1513),#1115,.T.);
#8117=ADVANCED_FACE('',(#1514),#1116,.T.);
#8118=ADVANCED_FACE('',(#1515,#891),#1117,.T.);
#8119=ADVANCED_FACE('',(#1516,#892),#1118,.F.);
#8120=ADVANCED_FACE('',(#1517),#1119,.T.);
#8121=ADVANCED_FACE('',(#1518),#1120,.T.);
#8122=ADVANCED_FACE('',(#1519),#1121,.T.);
#8123=ADVANCED_FACE('',(#1520),#1122,.T.);
#8124=ADVANCED_FACE('',(#1521,#893,#894,#895,#896,#897,#898),#1123,.T.);
#8125=ADVANCED_FACE('',(#1522,#899,#900,#901,#902),#1124,.F.);
#8126=ADVANCED_FACE('',(#1523),#7774,.F.);
#8127=ADVANCED_FACE('',(#1524),#1125,.T.);
#8128=ADVANCED_FACE('',(#1525,#903),#1126,.T.);
#8129=ADVANCED_FACE('',(#1526),#7775,.T.);
#8130=ADVANCED_FACE('',(#1527),#1127,.F.);
#8131=ADVANCED_FACE('',(#1528),#7776,.T.);
#8132=ADVANCED_FACE('',(#1529,#904),#1128,.T.);
#8133=ADVANCED_FACE('',(#1530),#7777,.F.);
#8134=ADVANCED_FACE('',(#1531),#7778,.T.);
#8135=ADVANCED_FACE('',(#1532,#905),#1129,.T.);
#8136=ADVANCED_FACE('',(#1533,#906),#1130,.F.);
#8137=ADVANCED_FACE('',(#1534),#7779,.F.);
#8138=ADVANCED_FACE('',(#1535),#7780,.T.);
#8139=ADVANCED_FACE('',(#1536,#907),#1131,.T.);
#8140=ADVANCED_FACE('',(#1537,#908),#1132,.F.);
#8141=ADVANCED_FACE('',(#1538),#7781,.F.);
#8142=ADVANCED_FACE('',(#1539),#7782,.T.);
#8143=ADVANCED_FACE('',(#1540,#909),#1133,.T.);
#8144=ADVANCED_FACE('',(#1541,#910),#1134,.F.);
#8145=ADVANCED_FACE('',(#1542),#7783,.F.);
#8146=ADVANCED_FACE('',(#1543),#7784,.F.);
#8147=ADVANCED_FACE('',(#1544),#7785,.F.);
#8148=ADVANCED_FACE('',(#1545),#7786,.F.);
#8149=ADVANCED_FACE('',(#1546),#7787,.F.);
#8150=ADVANCED_FACE('',(#1547),#7788,.F.);
#8151=ADVANCED_FACE('',(#1548),#1135,.T.);
#8152=ADVANCED_FACE('',(#1549),#1136,.T.);
#8153=ADVANCED_FACE('',(#1550),#1137,.T.);
#8154=ADVANCED_FACE('',(#1551,#911),#1138,.T.);
#8155=ADVANCED_FACE('',(#1552,#912),#1139,.F.);
#8156=ADVANCED_FACE('',(#1553),#1140,.T.);
#8157=ADVANCED_FACE('',(#1554),#1141,.T.);
#8158=ADVANCED_FACE('',(#1555),#1142,.T.);
#8159=ADVANCED_FACE('',(#1556,#913),#1143,.T.);
#8160=ADVANCED_FACE('',(#1557,#914),#1144,.F.);
#8161=ADVANCED_FACE('',(#1558),#1145,.T.);
#8162=ADVANCED_FACE('',(#1559),#1146,.T.);
#8163=ADVANCED_FACE('',(#1560),#1147,.T.);
#8164=ADVANCED_FACE('',(#1561),#1148,.T.);
#8165=ADVANCED_FACE('',(#1562,#915,#916,#917,#918,#919,#920),#1149,.T.);
#8166=ADVANCED_FACE('',(#1563,#921,#922,#923,#924),#1150,.F.);
#8167=ADVANCED_FACE('',(#1564),#7789,.F.);
#8168=ADVANCED_FACE('',(#1565),#1151,.T.);
#8169=ADVANCED_FACE('',(#1566,#925),#1152,.T.);
#8170=ADVANCED_FACE('',(#1567),#7790,.T.);
#8171=ADVANCED_FACE('',(#1568),#1153,.F.);
#8172=ADVANCED_FACE('',(#1569),#7791,.T.);
#8173=ADVANCED_FACE('',(#1570,#926),#1154,.T.);
#8174=ADVANCED_FACE('',(#1571),#7792,.F.);
#8175=ADVANCED_FACE('',(#1572),#7793,.T.);
#8176=ADVANCED_FACE('',(#1573,#927),#1155,.T.);
#8177=ADVANCED_FACE('',(#1574,#928),#1156,.F.);
#8178=ADVANCED_FACE('',(#1575),#7794,.F.);
#8179=ADVANCED_FACE('',(#1576),#7795,.T.);
#8180=ADVANCED_FACE('',(#1577,#929),#1157,.T.);
#8181=ADVANCED_FACE('',(#1578,#930),#1158,.F.);
#8182=ADVANCED_FACE('',(#1579),#7796,.F.);
#8183=ADVANCED_FACE('',(#1580),#7797,.T.);
#8184=ADVANCED_FACE('',(#1581,#931),#1159,.T.);
#8185=ADVANCED_FACE('',(#1582,#932),#1160,.F.);
#8186=ADVANCED_FACE('',(#1583),#7798,.F.);
#8187=ADVANCED_FACE('',(#1584),#7799,.F.);
#8188=ADVANCED_FACE('',(#1585),#7800,.F.);
#8189=ADVANCED_FACE('',(#1586),#7801,.F.);
#8190=ADVANCED_FACE('',(#1587),#7802,.F.);
#8191=ADVANCED_FACE('',(#1588),#7803,.F.);
#8192=ADVANCED_FACE('',(#1589),#1161,.T.);
#8193=ADVANCED_FACE('',(#1590),#1162,.T.);
#8194=ADVANCED_FACE('',(#1591),#1163,.T.);
#8195=ADVANCED_FACE('',(#1592,#933),#1164,.T.);
#8196=ADVANCED_FACE('',(#1593,#934),#1165,.F.);
#8197=ADVANCED_FACE('',(#1594),#1166,.T.);
#8198=ADVANCED_FACE('',(#1595),#1167,.T.);
#8199=ADVANCED_FACE('',(#1596),#1168,.T.);
#8200=ADVANCED_FACE('',(#1597,#935),#1169,.T.);
#8201=ADVANCED_FACE('',(#1598,#936),#1170,.F.);
#8202=ADVANCED_FACE('',(#1599),#1171,.T.);
#8203=ADVANCED_FACE('',(#1600),#1172,.T.);
#8204=ADVANCED_FACE('',(#1601),#1173,.T.);
#8205=ADVANCED_FACE('',(#1602),#1174,.T.);
#8206=ADVANCED_FACE('',(#1603,#937,#938,#939,#940,#941,#942),#1175,.T.);
#8207=ADVANCED_FACE('',(#1604,#943,#944,#945,#946),#1176,.F.);
#8208=ADVANCED_FACE('',(#1605),#7804,.F.);
#8209=ADVANCED_FACE('',(#1606),#1177,.T.);
#8210=ADVANCED_FACE('',(#1607,#947),#1178,.T.);
#8211=ADVANCED_FACE('',(#1608),#7805,.T.);
#8212=ADVANCED_FACE('',(#1609),#1179,.F.);
#8213=ADVANCED_FACE('',(#1610),#7806,.T.);
#8214=ADVANCED_FACE('',(#1611,#948),#1180,.T.);
#8215=ADVANCED_FACE('',(#1612),#7807,.F.);
#8216=ADVANCED_FACE('',(#1613),#7808,.T.);
#8217=ADVANCED_FACE('',(#1614,#949),#1181,.T.);
#8218=ADVANCED_FACE('',(#1615,#950),#1182,.F.);
#8219=ADVANCED_FACE('',(#1616),#7809,.F.);
#8220=ADVANCED_FACE('',(#1617),#7810,.T.);
#8221=ADVANCED_FACE('',(#1618,#951),#1183,.T.);
#8222=ADVANCED_FACE('',(#1619,#952),#1184,.F.);
#8223=ADVANCED_FACE('',(#1620),#7811,.F.);
#8224=ADVANCED_FACE('',(#1621),#7812,.T.);
#8225=ADVANCED_FACE('',(#1622,#953),#1185,.T.);
#8226=ADVANCED_FACE('',(#1623,#954),#1186,.F.);
#8227=ADVANCED_FACE('',(#1624),#1187,.F.);
#8228=ADVANCED_FACE('',(#1625),#1188,.F.);
#8229=ADVANCED_FACE('',(#1626),#1189,.F.);
#8230=ADVANCED_FACE('',(#1627),#1190,.F.);
#8231=ADVANCED_FACE('',(#1628),#1191,.F.);
#8232=ADVANCED_FACE('',(#1629),#1192,.F.);
#8233=ADVANCED_FACE('',(#1630),#1193,.F.);
#8234=ADVANCED_FACE('',(#1631),#1194,.F.);
#8235=ADVANCED_FACE('',(#1632),#1195,.F.);
#8236=ADVANCED_FACE('',(#1633),#1196,.T.);
#8237=ADVANCED_FACE('',(#1634),#489,.T.);
#8238=ADVANCED_FACE('',(#1635),#7813,.T.);
#8239=ADVANCED_FACE('',(#1636),#490,.T.);
#8240=ADVANCED_FACE('',(#1637,#955),#1197,.T.);
#8241=ADVANCED_FACE('',(#1638),#491,.T.);
#8242=ADVANCED_FACE('',(#1639),#7814,.T.);
#8243=ADVANCED_FACE('',(#1640),#1198,.F.);
#8244=ADVANCED_FACE('',(#1641),#1199,.F.);
#8245=ADVANCED_FACE('',(#1642),#1200,.F.);
#8246=ADVANCED_FACE('',(#1643),#1201,.F.);
#8247=ADVANCED_FACE('',(#1644),#1202,.F.);
#8248=ADVANCED_FACE('',(#1645),#1203,.F.);
#8249=ADVANCED_FACE('',(#1646),#1204,.F.);
#8250=ADVANCED_FACE('',(#1647),#1205,.F.);
#8251=ADVANCED_FACE('',(#1648),#1206,.F.);
#8252=ADVANCED_FACE('',(#1649),#1207,.T.);
#8253=ADVANCED_FACE('',(#1650),#492,.T.);
#8254=ADVANCED_FACE('',(#1651),#7815,.T.);
#8255=ADVANCED_FACE('',(#1652),#493,.T.);
#8256=ADVANCED_FACE('',(#1653,#956),#1208,.T.);
#8257=ADVANCED_FACE('',(#1654),#494,.T.);
#8258=ADVANCED_FACE('',(#1655),#7816,.T.);
#8259=ADVANCED_FACE('',(#1656),#7817,.F.);
#8260=ADVANCED_FACE('',(#1657),#7818,.T.);
#8261=ADVANCED_FACE('',(#1658,#957),#1209,.T.);
#8262=ADVANCED_FACE('',(#1659,#958),#1210,.F.);
#8263=ADVANCED_FACE('',(#1660),#7819,.F.);
#8264=ADVANCED_FACE('',(#1661),#7820,.T.);
#8265=ADVANCED_FACE('',(#1662,#959),#1211,.T.);
#8266=ADVANCED_FACE('',(#1663,#960),#1212,.F.);
#8267=ADVANCED_FACE('',(#1664),#7821,.F.);
#8268=ADVANCED_FACE('',(#1665),#7822,.T.);
#8269=ADVANCED_FACE('',(#1666,#961),#1213,.T.);
#8270=ADVANCED_FACE('',(#1667,#962),#1214,.F.);
#8271=ADVANCED_FACE('',(#1668),#7823,.F.);
#8272=ADVANCED_FACE('',(#1669),#7824,.T.);
#8273=ADVANCED_FACE('',(#1670,#963),#1215,.T.);
#8274=ADVANCED_FACE('',(#1671,#964),#1216,.F.);
#8275=ADVANCED_FACE('',(#1672),#7825,.F.);
#8276=ADVANCED_FACE('',(#1673),#7826,.T.);
#8277=ADVANCED_FACE('',(#1674,#965),#1217,.T.);
#8278=ADVANCED_FACE('',(#1675,#966),#1218,.F.);
#8279=ADVANCED_FACE('',(#1676),#7827,.F.);
#8280=ADVANCED_FACE('',(#1677),#7828,.T.);
#8281=ADVANCED_FACE('',(#1678,#967),#1219,.T.);
#8282=ADVANCED_FACE('',(#1679,#968),#1220,.F.);
#8283=ADVANCED_FACE('',(#1680),#7829,.F.);
#8284=ADVANCED_FACE('',(#1681),#7830,.T.);
#8285=ADVANCED_FACE('',(#1682,#969),#1221,.T.);
#8286=ADVANCED_FACE('',(#1683,#970),#1222,.F.);
#8287=ADVANCED_FACE('',(#1684),#7831,.F.);
#8288=ADVANCED_FACE('',(#1685),#7832,.T.);
#8289=ADVANCED_FACE('',(#1686,#971),#1223,.T.);
#8290=ADVANCED_FACE('',(#1687,#972),#1224,.F.);
#8291=ADVANCED_FACE('',(#1688),#7833,.F.);
#8292=ADVANCED_FACE('',(#1689),#7834,.T.);
#8293=ADVANCED_FACE('',(#1690,#973),#1225,.T.);
#8294=ADVANCED_FACE('',(#1691,#974),#1226,.F.);
#8295=ADVANCED_FACE('',(#1692),#7835,.F.);
#8296=ADVANCED_FACE('',(#1693),#7836,.T.);
#8297=ADVANCED_FACE('',(#1694,#975),#1227,.T.);
#8298=ADVANCED_FACE('',(#1695,#976),#1228,.F.);
#8299=ADVANCED_FACE('',(#1696),#7837,.F.);
#8300=ADVANCED_FACE('',(#1697),#7838,.T.);
#8301=ADVANCED_FACE('',(#1698,#977),#1229,.T.);
#8302=ADVANCED_FACE('',(#1699,#978),#1230,.F.);
#8303=ADVANCED_FACE('',(#1700),#7839,.F.);
#8304=ADVANCED_FACE('',(#1701),#7840,.T.);
#8305=ADVANCED_FACE('',(#1702,#979),#1231,.T.);
#8306=ADVANCED_FACE('',(#1703,#980),#1232,.F.);
#8307=ADVANCED_FACE('',(#1704),#474,.F.);
#8308=ADVANCED_FACE('',(#1705),#7841,.T.);
#8309=ADVANCED_FACE('',(#1706),#7842,.F.);
#8310=ADVANCED_FACE('',(#1707),#495,.F.);
#8311=ADVANCED_FACE('',(#1708,#981),#1233,.T.);
#8312=ADVANCED_FACE('',(#1709),#7843,.T.);
#8313=ADVANCED_FACE('',(#1710,#982),#1234,.T.);
#8314=ADVANCED_FACE('',(#1711),#496,.F.);
#8315=ADVANCED_FACE('',(#1712),#475,.F.);
#8316=ADVANCED_FACE('',(#1713),#7844,.F.);
#8317=ADVANCED_FACE('',(#1714,#983),#1235,.T.);
#8318=ADVANCED_FACE('',(#1715),#497,.T.);
#8319=ADVANCED_FACE('',(#1716),#7845,.T.);
#8320=ADVANCED_FACE('',(#1717),#498,.T.);
#8321=ADVANCED_FACE('',(#1718,#984),#1236,.T.);
#8322=ADVANCED_FACE('',(#1719),#7846,.F.);
#8323=ADVANCED_FACE('',(#1720),#456,.T.);
#8324=ADVANCED_FACE('',(#1721),#457,.T.);
#8325=ADVANCED_FACE('',(#1722),#458,.T.);
#8326=ADVANCED_FACE('',(#1723),#459,.T.);
#8327=ADVANCED_FACE('',(#1724),#460,.T.);
#8328=ADVANCED_FACE('',(#1725),#461,.T.);
#8329=ADVANCED_FACE('',(#1726),#462,.T.);
#8330=ADVANCED_FACE('',(#1727),#463,.T.);
#8331=ADVANCED_FACE('',(#1728),#464,.F.);
#8332=ADVANCED_FACE('',(#1729),#7847,.T.);
#8333=ADVANCED_FACE('',(#1730),#1237,.T.);
#8334=ADVANCED_FACE('',(#1731),#465,.F.);
#8335=ADVANCED_FACE('',(#1732),#1238,.T.);
#8336=ADVANCED_FACE('',(#1733),#466,.F.);
#8337=ADVANCED_FACE('',(#1734),#1239,.T.);
#8338=ADVANCED_FACE('',(#1735),#467,.F.);
#8339=ADVANCED_FACE('',(#1736),#1240,.T.);
#8340=ADVANCED_FACE('',(#1737),#468,.F.);
#8341=ADVANCED_FACE('',(#1738),#1241,.T.);
#8342=ADVANCED_FACE('',(#1739),#469,.F.);
#8343=ADVANCED_FACE('',(#1740),#1242,.T.);
#8344=ADVANCED_FACE('',(#1741),#470,.F.);
#8345=ADVANCED_FACE('',(#1742),#7848,.F.);
#8346=ADVANCED_FACE('',(#1743),#1243,.T.);
#8347=ADVANCED_FACE('',(#1744),#471,.F.);
#8348=ADVANCED_FACE('',(#1745,#985),#1244,.T.);
#8349=ADVANCED_FACE('',(#1746),#1245,.T.);
#8350=ADVANCED_FACE('',(#1747,#986),#1246,.T.);
#8351=ADVANCED_FACE('',(#1748),#7849,.T.);
#8352=ADVANCED_FACE('',(#1749,#987),#1247,.T.);
#8353=ADVANCED_FACE('',(#1750),#7850,.F.);
#8354=ADVANCED_FACE('',(#1751,#988),#1248,.T.);
#8355=ADVANCED_FACE('',(#1752),#7851,.T.);
#8356=ADVANCED_FACE('',(#1753,#989),#1249,.T.);
#8357=ADVANCED_FACE('',(#1754),#7852,.F.);
#8358=CLOSED_SHELL('',(#7853,#7854,#7855,#7856,#7857,#7858,#7859,#7860,
#7861,#7862,#7863,#7864,#7865,#7866,#7867,#7868,#7869,#7870,#7871,#7872,
#7873,#7874,#7875,#7876,#7877,#7878));
#8359=CLOSED_SHELL('',(#7879,#7880,#7881,#7882,#7883,#7884,#7885,#7886,
#7887,#7888,#7889,#7890,#7891,#7892,#7893,#7894,#7895,#7896,#7897,#7898,
#7899,#7900,#7901,#7902,#7903,#7904,#7905,#7906,#7907,#7908));
#8360=CLOSED_SHELL('',(#7909,#7910,#7911,#7912,#7913,#7914,#7915,#7916,
#7917,#7918));
#8361=CLOSED_SHELL('',(#7919,#7920,#7921,#7922,#7923,#7924,#7925,#7926));
#8362=CLOSED_SHELL('',(#7927,#7928,#7929,#7930,#7931,#7932,#7933,#7934));
#8363=CLOSED_SHELL('',(#7935,#7936,#7937,#7938,#7939,#7940,#7941,#7942));
#8364=CLOSED_SHELL('',(#7943,#7944,#7945,#7946,#7947,#7948,#7949,#7950));
#8365=CLOSED_SHELL('',(#7951));
#8366=CLOSED_SHELL('',(#7952));
#8367=CLOSED_SHELL('',(#7953));
#8368=CLOSED_SHELL('',(#7954));
#8369=CLOSED_SHELL('',(#7955));
#8370=CLOSED_SHELL('',(#7956));
#8371=CLOSED_SHELL('',(#7957));
#8372=CLOSED_SHELL('',(#7958));
#8373=CLOSED_SHELL('',(#7959));
#8374=CLOSED_SHELL('',(#7960,#7961,#7962,#7963,#7964,#7965,#7966,#7967,
#7968,#7969,#7970,#7971,#7972,#7973,#7974,#7975,#7976,#7977,#7978,#7979,
#7980));
#8375=CLOSED_SHELL('',(#7981,#7982,#7983,#7984));
#8376=CLOSED_SHELL('',(#7985,#7986,#7987,#7988));
#8377=CLOSED_SHELL('',(#7989,#7990,#7991,#7992,#7993,#7994));
#8378=CLOSED_SHELL('',(#7995,#7996,#7997,#7998,#7999,#8000));
#8379=CLOSED_SHELL('',(#8001,#8002,#8003,#8004,#8005,#8006,#8007,#8008,
#8009,#8010,#8011));
#8380=CLOSED_SHELL('',(#8012,#8013,#8014,#8015,#8016,#8017,#8018,#8019,
#8020,#8021,#8022,#8023,#8024,#8025,#8026));
#8381=CLOSED_SHELL('',(#8027,#8028,#8029,#8030,#8031,#8032,#8033));
#8382=CLOSED_SHELL('',(#8034,#8035,#8036,#8037,#8038,#8039,#8040,#8041,
#8042));
#8383=CLOSED_SHELL('',(#8043,#8044,#8045,#8046,#8047,#8048,#8049,#8050));
#8384=CLOSED_SHELL('',(#8051,#8052,#8053,#8054,#8055,#8056,#8057,#8058,
#8059,#8060,#8061,#8062));
#8385=CLOSED_SHELL('',(#8063,#8064,#8065,#8066,#8067,#8068,#8069,#8070,
#8071,#8072,#8073,#8074,#8075,#8076,#8077,#8078,#8079,#8080,#8081,#8082,
#8083,#8084));
#8386=CLOSED_SHELL('',(#8085,#8086,#8087,#8088,#8089,#8090,#8091));
#8387=CLOSED_SHELL('',(#8092,#8093,#8094,#8095));
#8388=CLOSED_SHELL('',(#8096,#8097,#8098,#8099));
#8389=CLOSED_SHELL('',(#8100,#8101,#8102,#8103));
#8390=CLOSED_SHELL('',(#8104,#8105,#8106,#8107,#8108,#8109,#8110,#8111,
#8112,#8113,#8114,#8115,#8116,#8117,#8118,#8119,#8120,#8121,#8122,#8123,
#8124,#8125));
#8391=CLOSED_SHELL('',(#8126,#8127,#8128,#8129,#8130,#8131,#8132));
#8392=CLOSED_SHELL('',(#8133,#8134,#8135,#8136));
#8393=CLOSED_SHELL('',(#8137,#8138,#8139,#8140));
#8394=CLOSED_SHELL('',(#8141,#8142,#8143,#8144));
#8395=CLOSED_SHELL('',(#8145,#8146,#8147,#8148,#8149,#8150,#8151,#8152,
#8153,#8154,#8155,#8156,#8157,#8158,#8159,#8160,#8161,#8162,#8163,#8164,
#8165,#8166));
#8396=CLOSED_SHELL('',(#8167,#8168,#8169,#8170,#8171,#8172,#8173));
#8397=CLOSED_SHELL('',(#8174,#8175,#8176,#8177));
#8398=CLOSED_SHELL('',(#8178,#8179,#8180,#8181));
#8399=CLOSED_SHELL('',(#8182,#8183,#8184,#8185));
#8400=CLOSED_SHELL('',(#8186,#8187,#8188,#8189,#8190,#8191,#8192,#8193,
#8194,#8195,#8196,#8197,#8198,#8199,#8200,#8201,#8202,#8203,#8204,#8205,
#8206,#8207));
#8401=CLOSED_SHELL('',(#8208,#8209,#8210,#8211,#8212,#8213,#8214));
#8402=CLOSED_SHELL('',(#8215,#8216,#8217,#8218));
#8403=CLOSED_SHELL('',(#8219,#8220,#8221,#8222));
#8404=CLOSED_SHELL('',(#8223,#8224,#8225,#8226));
#8405=CLOSED_SHELL('',(#8227,#8228,#8229,#8230,#8231,#8232,#8233,#8234));
#8406=CLOSED_SHELL('',(#8235,#8236,#8237,#8238,#8239,#8240,#8241,#8242));
#8407=CLOSED_SHELL('',(#8243,#8244,#8245,#8246,#8247,#8248,#8249,#8250));
#8408=CLOSED_SHELL('',(#8251,#8252,#8253,#8254,#8255,#8256,#8257,#8258));
#8409=CLOSED_SHELL('',(#8259,#8260,#8261,#8262));
#8410=CLOSED_SHELL('',(#8263,#8264,#8265,#8266));
#8411=CLOSED_SHELL('',(#8267,#8268,#8269,#8270));
#8412=CLOSED_SHELL('',(#8271,#8272,#8273,#8274));
#8413=CLOSED_SHELL('',(#8275,#8276,#8277,#8278));
#8414=CLOSED_SHELL('',(#8279,#8280,#8281,#8282));
#8415=CLOSED_SHELL('',(#8283,#8284,#8285,#8286));
#8416=CLOSED_SHELL('',(#8287,#8288,#8289,#8290));
#8417=CLOSED_SHELL('',(#8291,#8292,#8293,#8294));
#8418=CLOSED_SHELL('',(#8295,#8296,#8297,#8298));
#8419=CLOSED_SHELL('',(#8299,#8300,#8301,#8302));
#8420=CLOSED_SHELL('',(#8303,#8304,#8305,#8306));
#8421=CLOSED_SHELL('',(#8307,#8308,#8309,#8310,#8311,#8312,#8313,#8314));
#8422=CLOSED_SHELL('',(#8315,#8316,#8317,#8318,#8319,#8320,#8321,#8322));
#8423=CLOSED_SHELL('',(#8323));
#8424=CLOSED_SHELL('',(#8324));
#8425=CLOSED_SHELL('',(#8325));
#8426=CLOSED_SHELL('',(#8326));
#8427=CLOSED_SHELL('',(#8327));
#8428=CLOSED_SHELL('',(#8328));
#8429=CLOSED_SHELL('',(#8329));
#8430=CLOSED_SHELL('',(#8330));
#8431=CLOSED_SHELL('',(#8331,#8332,#8333,#8334,#8335,#8336,#8337,#8338,
#8339,#8340,#8341,#8342,#8343,#8344,#8345,#8346,#8347,#8348,#8349));
#8432=CLOSED_SHELL('',(#8350,#8351,#8352,#8353));
#8433=CLOSED_SHELL('',(#8354,#8355,#8356,#8357));
#8434=DERIVED_UNIT_ELEMENT(#8544,1.);
#8435=DERIVED_UNIT_ELEMENT(#16283,-3.);
#8436=DERIVED_UNIT_ELEMENT(#8544,1.);
#8437=DERIVED_UNIT_ELEMENT(#16283,-3.);
#8438=DERIVED_UNIT_ELEMENT(#8544,1.);
#8439=DERIVED_UNIT_ELEMENT(#16283,-3.);
#8440=DERIVED_UNIT_ELEMENT(#8544,1.);
#8441=DERIVED_UNIT_ELEMENT(#16283,-3.);
#8442=DERIVED_UNIT_ELEMENT(#8544,1.);
#8443=DERIVED_UNIT_ELEMENT(#16283,-3.);
#8444=DERIVED_UNIT_ELEMENT(#8544,1.);
#8445=DERIVED_UNIT_ELEMENT(#16283,-3.);
#8446=DERIVED_UNIT_ELEMENT(#8544,1.);
#8447=DERIVED_UNIT_ELEMENT(#16283,-3.);
#8448=DERIVED_UNIT_ELEMENT(#8544,1.);
#8449=DERIVED_UNIT_ELEMENT(#16283,-3.);
#8450=DERIVED_UNIT_ELEMENT(#8544,1.);
#8451=DERIVED_UNIT_ELEMENT(#16283,-3.);
#8452=DERIVED_UNIT_ELEMENT(#8544,1.);
#8453=DERIVED_UNIT_ELEMENT(#16283,-3.);
#8454=DERIVED_UNIT_ELEMENT(#8544,1.);
#8455=DERIVED_UNIT_ELEMENT(#16283,-3.);
#8456=DERIVED_UNIT_ELEMENT(#8544,1.);
#8457=DERIVED_UNIT_ELEMENT(#16283,-3.);
#8458=DERIVED_UNIT_ELEMENT(#8544,1.);
#8459=DERIVED_UNIT_ELEMENT(#16283,-3.);
#8460=DERIVED_UNIT_ELEMENT(#8544,1.);
#8461=DERIVED_UNIT_ELEMENT(#16283,-3.);
#8462=DERIVED_UNIT_ELEMENT(#8544,1.);
#8463=DERIVED_UNIT_ELEMENT(#16283,-3.);
#8464=DERIVED_UNIT_ELEMENT(#8544,1.);
#8465=DERIVED_UNIT_ELEMENT(#16283,-3.);
#8466=DERIVED_UNIT_ELEMENT(#8544,1.);
#8467=DERIVED_UNIT_ELEMENT(#16283,-3.);
#8468=DERIVED_UNIT_ELEMENT(#8544,1.);
#8469=DERIVED_UNIT_ELEMENT(#16283,-3.);
#8470=DERIVED_UNIT_ELEMENT(#8544,1.);
#8471=DERIVED_UNIT_ELEMENT(#16283,-3.);
#8472=DERIVED_UNIT_ELEMENT(#8544,1.);
#8473=DERIVED_UNIT_ELEMENT(#16283,-3.);
#8474=DERIVED_UNIT_ELEMENT(#8544,1.);
#8475=DERIVED_UNIT_ELEMENT(#16283,-3.);
#8476=DERIVED_UNIT_ELEMENT(#8544,1.);
#8477=DERIVED_UNIT_ELEMENT(#16283,-3.);
#8478=DERIVED_UNIT_ELEMENT(#8544,1.);
#8479=DERIVED_UNIT_ELEMENT(#16283,-3.);
#8480=DERIVED_UNIT_ELEMENT(#8544,1.);
#8481=DERIVED_UNIT_ELEMENT(#16283,-3.);
#8482=DERIVED_UNIT_ELEMENT(#8544,1.);
#8483=DERIVED_UNIT_ELEMENT(#16283,-3.);
#8484=DERIVED_UNIT_ELEMENT(#8544,1.);
#8485=DERIVED_UNIT_ELEMENT(#16283,-3.);
#8486=DERIVED_UNIT_ELEMENT(#8544,1.);
#8487=DERIVED_UNIT_ELEMENT(#16283,-3.);
#8488=DERIVED_UNIT_ELEMENT(#8544,1.);
#8489=DERIVED_UNIT_ELEMENT(#16283,-3.);
#8490=DERIVED_UNIT_ELEMENT(#8544,1.);
#8491=DERIVED_UNIT_ELEMENT(#16283,-3.);
#8492=DERIVED_UNIT_ELEMENT(#8544,1.);
#8493=DERIVED_UNIT_ELEMENT(#16283,-3.);
#8494=DERIVED_UNIT_ELEMENT(#8544,1.);
#8495=DERIVED_UNIT_ELEMENT(#16283,-3.);
#8496=DERIVED_UNIT_ELEMENT(#8544,1.);
#8497=DERIVED_UNIT_ELEMENT(#16283,-3.);
#8498=DERIVED_UNIT_ELEMENT(#8544,1.);
#8499=DERIVED_UNIT_ELEMENT(#16283,-3.);
#8500=DERIVED_UNIT_ELEMENT(#8544,1.);
#8501=DERIVED_UNIT_ELEMENT(#16283,-3.);
#8502=DERIVED_UNIT_ELEMENT(#8544,1.);
#8503=DERIVED_UNIT_ELEMENT(#16283,-3.);
#8504=DERIVED_UNIT_ELEMENT(#8544,1.);
#8505=DERIVED_UNIT_ELEMENT(#16283,-3.);
#8506=DERIVED_UNIT_ELEMENT(#8544,1.);
#8507=DERIVED_UNIT_ELEMENT(#16283,-3.);
#8508=DERIVED_UNIT_ELEMENT(#8544,1.);
#8509=DERIVED_UNIT_ELEMENT(#16283,-3.);
#8510=DERIVED_UNIT_ELEMENT(#8544,1.);
#8511=DERIVED_UNIT_ELEMENT(#16283,-3.);
#8512=DERIVED_UNIT_ELEMENT(#8544,1.);
#8513=DERIVED_UNIT_ELEMENT(#16283,-3.);
#8514=DERIVED_UNIT_ELEMENT(#8544,1.);
#8515=DERIVED_UNIT_ELEMENT(#16283,-3.);
#8516=DERIVED_UNIT_ELEMENT(#8544,1.);
#8517=DERIVED_UNIT_ELEMENT(#16283,-3.);
#8518=DERIVED_UNIT_ELEMENT(#8544,1.);
#8519=DERIVED_UNIT_ELEMENT(#16283,-3.);
#8520=DERIVED_UNIT_ELEMENT(#8544,1.);
#8521=DERIVED_UNIT_ELEMENT(#16283,-3.);
#8522=DERIVED_UNIT_ELEMENT(#8544,1.);
#8523=DERIVED_UNIT_ELEMENT(#16283,-3.);
#8524=DERIVED_UNIT_ELEMENT(#8544,1.);
#8525=DERIVED_UNIT_ELEMENT(#16283,-3.);
#8526=DERIVED_UNIT_ELEMENT(#8544,1.);
#8527=DERIVED_UNIT_ELEMENT(#16283,-3.);
#8528=DERIVED_UNIT_ELEMENT(#8544,1.);
#8529=DERIVED_UNIT_ELEMENT(#16283,-3.);
#8530=DERIVED_UNIT_ELEMENT(#8544,1.);
#8531=DERIVED_UNIT_ELEMENT(#16283,-3.);
#8532=DERIVED_UNIT_ELEMENT(#8544,1.);
#8533=DERIVED_UNIT_ELEMENT(#16283,-3.);
#8534=DERIVED_UNIT_ELEMENT(#8544,1.);
#8535=DERIVED_UNIT_ELEMENT(#16283,-3.);
#8536=DERIVED_UNIT_ELEMENT(#8544,1.);
#8537=DERIVED_UNIT_ELEMENT(#16283,-3.);
#8538=DERIVED_UNIT_ELEMENT(#8544,1.);
#8539=DERIVED_UNIT_ELEMENT(#16283,-3.);
#8540=DERIVED_UNIT_ELEMENT(#8544,1.);
#8541=DERIVED_UNIT_ELEMENT(#16283,-3.);
#8542=DERIVED_UNIT_ELEMENT(#8544,1.);
#8543=DERIVED_UNIT_ELEMENT(#16283,-3.);
#8544=(
MASS_UNIT()
NAMED_UNIT(*)
SI_UNIT(.KILO.,.GRAM.)
);
#8545=DERIVED_UNIT((#8434,#8435));
#8546=DERIVED_UNIT((#8436,#8437));
#8547=DERIVED_UNIT((#8438,#8439));
#8548=DERIVED_UNIT((#8440,#8441));
#8549=DERIVED_UNIT((#8442,#8443));
#8550=DERIVED_UNIT((#8444,#8445));
#8551=DERIVED_UNIT((#8446,#8447));
#8552=DERIVED_UNIT((#8448,#8449));
#8553=DERIVED_UNIT((#8450,#8451));
#8554=DERIVED_UNIT((#8452,#8453));
#8555=DERIVED_UNIT((#8454,#8455));
#8556=DERIVED_UNIT((#8456,#8457));
#8557=DERIVED_UNIT((#8458,#8459));
#8558=DERIVED_UNIT((#8460,#8461));
#8559=DERIVED_UNIT((#8462,#8463));
#8560=DERIVED_UNIT((#8464,#8465));
#8561=DERIVED_UNIT((#8466,#8467));
#8562=DERIVED_UNIT((#8468,#8469));
#8563=DERIVED_UNIT((#8470,#8471));
#8564=DERIVED_UNIT((#8472,#8473));
#8565=DERIVED_UNIT((#8474,#8475));
#8566=DERIVED_UNIT((#8476,#8477));
#8567=DERIVED_UNIT((#8478,#8479));
#8568=DERIVED_UNIT((#8480,#8481));
#8569=DERIVED_UNIT((#8482,#8483));
#8570=DERIVED_UNIT((#8484,#8485));
#8571=DERIVED_UNIT((#8486,#8487));
#8572=DERIVED_UNIT((#8488,#8489));
#8573=DERIVED_UNIT((#8490,#8491));
#8574=DERIVED_UNIT((#8492,#8493));
#8575=DERIVED_UNIT((#8494,#8495));
#8576=DERIVED_UNIT((#8496,#8497));
#8577=DERIVED_UNIT((#8498,#8499));
#8578=DERIVED_UNIT((#8500,#8501));
#8579=DERIVED_UNIT((#8502,#8503));
#8580=DERIVED_UNIT((#8504,#8505));
#8581=DERIVED_UNIT((#8506,#8507));
#8582=DERIVED_UNIT((#8508,#8509));
#8583=DERIVED_UNIT((#8510,#8511));
#8584=DERIVED_UNIT((#8512,#8513));
#8585=DERIVED_UNIT((#8514,#8515));
#8586=DERIVED_UNIT((#8516,#8517));
#8587=DERIVED_UNIT((#8518,#8519));
#8588=DERIVED_UNIT((#8520,#8521));
#8589=DERIVED_UNIT((#8522,#8523));
#8590=DERIVED_UNIT((#8524,#8525));
#8591=DERIVED_UNIT((#8526,#8527));
#8592=DERIVED_UNIT((#8528,#8529));
#8593=DERIVED_UNIT((#8530,#8531));
#8594=DERIVED_UNIT((#8532,#8533));
#8595=DERIVED_UNIT((#8534,#8535));
#8596=DERIVED_UNIT((#8536,#8537));
#8597=DERIVED_UNIT((#8538,#8539));
#8598=DERIVED_UNIT((#8540,#8541));
#8599=DERIVED_UNIT((#8542,#8543));
#8600=MEASURE_REPRESENTATION_ITEM('density measure',
POSITIVE_RATIO_MEASURE(7850.),#8545);
#8601=MEASURE_REPRESENTATION_ITEM('density measure',
POSITIVE_RATIO_MEASURE(7850.),#8546);
#8602=MEASURE_REPRESENTATION_ITEM('density measure',
POSITIVE_RATIO_MEASURE(7850.),#8547);
#8603=MEASURE_REPRESENTATION_ITEM('density measure',
POSITIVE_RATIO_MEASURE(7850.),#8548);
#8604=MEASURE_REPRESENTATION_ITEM('density measure',
POSITIVE_RATIO_MEASURE(7850.),#8549);
#8605=MEASURE_REPRESENTATION_ITEM('density measure',
POSITIVE_RATIO_MEASURE(7850.),#8550);
#8606=MEASURE_REPRESENTATION_ITEM('density measure',
POSITIVE_RATIO_MEASURE(7850.),#8551);
#8607=MEASURE_REPRESENTATION_ITEM('density measure',
POSITIVE_RATIO_MEASURE(7850.),#8552);
#8608=MEASURE_REPRESENTATION_ITEM('density measure',
POSITIVE_RATIO_MEASURE(7850.),#8553);
#8609=MEASURE_REPRESENTATION_ITEM('density measure',
POSITIVE_RATIO_MEASURE(7850.),#8554);
#8610=MEASURE_REPRESENTATION_ITEM('density measure',
POSITIVE_RATIO_MEASURE(7850.),#8555);
#8611=MEASURE_REPRESENTATION_ITEM('density measure',
POSITIVE_RATIO_MEASURE(7850.),#8556);
#8612=MEASURE_REPRESENTATION_ITEM('density measure',
POSITIVE_RATIO_MEASURE(7850.),#8557);
#8613=MEASURE_REPRESENTATION_ITEM('density measure',
POSITIVE_RATIO_MEASURE(7850.),#8558);
#8614=MEASURE_REPRESENTATION_ITEM('density measure',
POSITIVE_RATIO_MEASURE(7850.),#8559);
#8615=MEASURE_REPRESENTATION_ITEM('density measure',
POSITIVE_RATIO_MEASURE(7850.),#8560);
#8616=MEASURE_REPRESENTATION_ITEM('density measure',
POSITIVE_RATIO_MEASURE(7850.),#8561);
#8617=MEASURE_REPRESENTATION_ITEM('density measure',
POSITIVE_RATIO_MEASURE(7850.),#8562);
#8618=MEASURE_REPRESENTATION_ITEM('density measure',
POSITIVE_RATIO_MEASURE(7850.),#8563);
#8619=MEASURE_REPRESENTATION_ITEM('density measure',
POSITIVE_RATIO_MEASURE(7850.),#8564);
#8620=MEASURE_REPRESENTATION_ITEM('density measure',
POSITIVE_RATIO_MEASURE(7850.),#8565);
#8621=MEASURE_REPRESENTATION_ITEM('density measure',
POSITIVE_RATIO_MEASURE(7850.),#8566);
#8622=MEASURE_REPRESENTATION_ITEM('density measure',
POSITIVE_RATIO_MEASURE(7850.),#8567);
#8623=MEASURE_REPRESENTATION_ITEM('density measure',
POSITIVE_RATIO_MEASURE(7850.),#8568);
#8624=MEASURE_REPRESENTATION_ITEM('density measure',
POSITIVE_RATIO_MEASURE(7850.),#8569);
#8625=MEASURE_REPRESENTATION_ITEM('density measure',
POSITIVE_RATIO_MEASURE(7850.),#8570);
#8626=MEASURE_REPRESENTATION_ITEM('density measure',
POSITIVE_RATIO_MEASURE(7850.),#8571);
#8627=MEASURE_REPRESENTATION_ITEM('density measure',
POSITIVE_RATIO_MEASURE(7850.),#8572);
#8628=MEASURE_REPRESENTATION_ITEM('density measure',
POSITIVE_RATIO_MEASURE(7850.),#8573);
#8629=MEASURE_REPRESENTATION_ITEM('density measure',
POSITIVE_RATIO_MEASURE(7850.),#8574);
#8630=MEASURE_REPRESENTATION_ITEM('density measure',
POSITIVE_RATIO_MEASURE(7850.),#8575);
#8631=MEASURE_REPRESENTATION_ITEM('density measure',
POSITIVE_RATIO_MEASURE(7850.),#8576);
#8632=MEASURE_REPRESENTATION_ITEM('density measure',
POSITIVE_RATIO_MEASURE(7850.),#8577);
#8633=MEASURE_REPRESENTATION_ITEM('density measure',
POSITIVE_RATIO_MEASURE(7850.),#8578);
#8634=MEASURE_REPRESENTATION_ITEM('density measure',
POSITIVE_RATIO_MEASURE(7850.),#8579);
#8635=MEASURE_REPRESENTATION_ITEM('density measure',
POSITIVE_RATIO_MEASURE(7850.),#8580);
#8636=MEASURE_REPRESENTATION_ITEM('density measure',
POSITIVE_RATIO_MEASURE(7850.),#8581);
#8637=MEASURE_REPRESENTATION_ITEM('density measure',
POSITIVE_RATIO_MEASURE(7850.),#8582);
#8638=MEASURE_REPRESENTATION_ITEM('density measure',
POSITIVE_RATIO_MEASURE(7850.),#8583);
#8639=MEASURE_REPRESENTATION_ITEM('density measure',
POSITIVE_RATIO_MEASURE(7850.),#8584);
#8640=MEASURE_REPRESENTATION_ITEM('density measure',
POSITIVE_RATIO_MEASURE(7850.),#8585);
#8641=MEASURE_REPRESENTATION_ITEM('density measure',
POSITIVE_RATIO_MEASURE(7850.),#8586);
#8642=MEASURE_REPRESENTATION_ITEM('density measure',
POSITIVE_RATIO_MEASURE(7850.),#8587);
#8643=MEASURE_REPRESENTATION_ITEM('density measure',
POSITIVE_RATIO_MEASURE(7850.),#8588);
#8644=MEASURE_REPRESENTATION_ITEM('density measure',
POSITIVE_RATIO_MEASURE(7850.),#8589);
#8645=MEASURE_REPRESENTATION_ITEM('density measure',
POSITIVE_RATIO_MEASURE(7850.),#8590);
#8646=MEASURE_REPRESENTATION_ITEM('density measure',
POSITIVE_RATIO_MEASURE(7850.),#8591);
#8647=MEASURE_REPRESENTATION_ITEM('density measure',
POSITIVE_RATIO_MEASURE(7850.),#8592);
#8648=MEASURE_REPRESENTATION_ITEM('density measure',
POSITIVE_RATIO_MEASURE(7850.),#8593);
#8649=MEASURE_REPRESENTATION_ITEM('density measure',
POSITIVE_RATIO_MEASURE(7850.),#8594);
#8650=MEASURE_REPRESENTATION_ITEM('density measure',
POSITIVE_RATIO_MEASURE(7850.),#8595);
#8651=MEASURE_REPRESENTATION_ITEM('density measure',
POSITIVE_RATIO_MEASURE(7850.),#8596);
#8652=MEASURE_REPRESENTATION_ITEM('density measure',
POSITIVE_RATIO_MEASURE(7850.),#8597);
#8653=MEASURE_REPRESENTATION_ITEM('density measure',
POSITIVE_RATIO_MEASURE(7850.),#8598);
#8654=MEASURE_REPRESENTATION_ITEM('density measure',
POSITIVE_RATIO_MEASURE(7850.),#8599);
#8655=PROPERTY_DEFINITION_REPRESENTATION(#8930,#8765);
#8656=PROPERTY_DEFINITION_REPRESENTATION(#8931,#8766);
#8657=PROPERTY_DEFINITION_REPRESENTATION(#8932,#8767);
#8658=PROPERTY_DEFINITION_REPRESENTATION(#8933,#8768);
#8659=PROPERTY_DEFINITION_REPRESENTATION(#8934,#8769);
#8660=PROPERTY_DEFINITION_REPRESENTATION(#8935,#8770);
#8661=PROPERTY_DEFINITION_REPRESENTATION(#8936,#8771);
#8662=PROPERTY_DEFINITION_REPRESENTATION(#8937,#8772);
#8663=PROPERTY_DEFINITION_REPRESENTATION(#8938,#8773);
#8664=PROPERTY_DEFINITION_REPRESENTATION(#8939,#8774);
#8665=PROPERTY_DEFINITION_REPRESENTATION(#8940,#8775);
#8666=PROPERTY_DEFINITION_REPRESENTATION(#8941,#8776);
#8667=PROPERTY_DEFINITION_REPRESENTATION(#8942,#8777);
#8668=PROPERTY_DEFINITION_REPRESENTATION(#8943,#8778);
#8669=PROPERTY_DEFINITION_REPRESENTATION(#8944,#8779);
#8670=PROPERTY_DEFINITION_REPRESENTATION(#8945,#8780);
#8671=PROPERTY_DEFINITION_REPRESENTATION(#8946,#8781);
#8672=PROPERTY_DEFINITION_REPRESENTATION(#8947,#8782);
#8673=PROPERTY_DEFINITION_REPRESENTATION(#8948,#8783);
#8674=PROPERTY_DEFINITION_REPRESENTATION(#8949,#8784);
#8675=PROPERTY_DEFINITION_REPRESENTATION(#8950,#8785);
#8676=PROPERTY_DEFINITION_REPRESENTATION(#8951,#8786);
#8677=PROPERTY_DEFINITION_REPRESENTATION(#8952,#8787);
#8678=PROPERTY_DEFINITION_REPRESENTATION(#8953,#8788);
#8679=PROPERTY_DEFINITION_REPRESENTATION(#8954,#8789);
#8680=PROPERTY_DEFINITION_REPRESENTATION(#8955,#8790);
#8681=PROPERTY_DEFINITION_REPRESENTATION(#8956,#8791);
#8682=PROPERTY_DEFINITION_REPRESENTATION(#8957,#8792);
#8683=PROPERTY_DEFINITION_REPRESENTATION(#8958,#8793);
#8684=PROPERTY_DEFINITION_REPRESENTATION(#8959,#8794);
#8685=PROPERTY_DEFINITION_REPRESENTATION(#8960,#8795);
#8686=PROPERTY_DEFINITION_REPRESENTATION(#8961,#8796);
#8687=PROPERTY_DEFINITION_REPRESENTATION(#8962,#8797);
#8688=PROPERTY_DEFINITION_REPRESENTATION(#8963,#8798);
#8689=PROPERTY_DEFINITION_REPRESENTATION(#8964,#8799);
#8690=PROPERTY_DEFINITION_REPRESENTATION(#8965,#8800);
#8691=PROPERTY_DEFINITION_REPRESENTATION(#8966,#8801);
#8692=PROPERTY_DEFINITION_REPRESENTATION(#8967,#8802);
#8693=PROPERTY_DEFINITION_REPRESENTATION(#8968,#8803);
#8694=PROPERTY_DEFINITION_REPRESENTATION(#8969,#8804);
#8695=PROPERTY_DEFINITION_REPRESENTATION(#8970,#8805);
#8696=PROPERTY_DEFINITION_REPRESENTATION(#8971,#8806);
#8697=PROPERTY_DEFINITION_REPRESENTATION(#8972,#8807);
#8698=PROPERTY_DEFINITION_REPRESENTATION(#8973,#8808);
#8699=PROPERTY_DEFINITION_REPRESENTATION(#8974,#8809);
#8700=PROPERTY_DEFINITION_REPRESENTATION(#8975,#8810);
#8701=PROPERTY_DEFINITION_REPRESENTATION(#8976,#8811);
#8702=PROPERTY_DEFINITION_REPRESENTATION(#8977,#8812);
#8703=PROPERTY_DEFINITION_REPRESENTATION(#8978,#8813);
#8704=PROPERTY_DEFINITION_REPRESENTATION(#8979,#8814);
#8705=PROPERTY_DEFINITION_REPRESENTATION(#8980,#8815);
#8706=PROPERTY_DEFINITION_REPRESENTATION(#8981,#8816);
#8707=PROPERTY_DEFINITION_REPRESENTATION(#8982,#8817);
#8708=PROPERTY_DEFINITION_REPRESENTATION(#8983,#8818);
#8709=PROPERTY_DEFINITION_REPRESENTATION(#8984,#8819);
#8710=PROPERTY_DEFINITION_REPRESENTATION(#8985,#8820);
#8711=PROPERTY_DEFINITION_REPRESENTATION(#8986,#8821);
#8712=PROPERTY_DEFINITION_REPRESENTATION(#8987,#8822);
#8713=PROPERTY_DEFINITION_REPRESENTATION(#8988,#8823);
#8714=PROPERTY_DEFINITION_REPRESENTATION(#8989,#8824);
#8715=PROPERTY_DEFINITION_REPRESENTATION(#8990,#8825);
#8716=PROPERTY_DEFINITION_REPRESENTATION(#8991,#8826);
#8717=PROPERTY_DEFINITION_REPRESENTATION(#8992,#8827);
#8718=PROPERTY_DEFINITION_REPRESENTATION(#8993,#8828);
#8719=PROPERTY_DEFINITION_REPRESENTATION(#8994,#8829);
#8720=PROPERTY_DEFINITION_REPRESENTATION(#8995,#8830);
#8721=PROPERTY_DEFINITION_REPRESENTATION(#8996,#8831);
#8722=PROPERTY_DEFINITION_REPRESENTATION(#8997,#8832);
#8723=PROPERTY_DEFINITION_REPRESENTATION(#8998,#8833);
#8724=PROPERTY_DEFINITION_REPRESENTATION(#8999,#8834);
#8725=PROPERTY_DEFINITION_REPRESENTATION(#9000,#8835);
#8726=PROPERTY_DEFINITION_REPRESENTATION(#9001,#8836);
#8727=PROPERTY_DEFINITION_REPRESENTATION(#9002,#8837);
#8728=PROPERTY_DEFINITION_REPRESENTATION(#9003,#8838);
#8729=PROPERTY_DEFINITION_REPRESENTATION(#9004,#8839);
#8730=PROPERTY_DEFINITION_REPRESENTATION(#9005,#8840);
#8731=PROPERTY_DEFINITION_REPRESENTATION(#9006,#8841);
#8732=PROPERTY_DEFINITION_REPRESENTATION(#9007,#8842);
#8733=PROPERTY_DEFINITION_REPRESENTATION(#9008,#8843);
#8734=PROPERTY_DEFINITION_REPRESENTATION(#9009,#8844);
#8735=PROPERTY_DEFINITION_REPRESENTATION(#9010,#8845);
#8736=PROPERTY_DEFINITION_REPRESENTATION(#9011,#8846);
#8737=PROPERTY_DEFINITION_REPRESENTATION(#9012,#8847);
#8738=PROPERTY_DEFINITION_REPRESENTATION(#9013,#8848);
#8739=PROPERTY_DEFINITION_REPRESENTATION(#9014,#8849);
#8740=PROPERTY_DEFINITION_REPRESENTATION(#9015,#8850);
#8741=PROPERTY_DEFINITION_REPRESENTATION(#9016,#8851);
#8742=PROPERTY_DEFINITION_REPRESENTATION(#9017,#8852);
#8743=PROPERTY_DEFINITION_REPRESENTATION(#9018,#8853);
#8744=PROPERTY_DEFINITION_REPRESENTATION(#9019,#8854);
#8745=PROPERTY_DEFINITION_REPRESENTATION(#9020,#8855);
#8746=PROPERTY_DEFINITION_REPRESENTATION(#9021,#8856);
#8747=PROPERTY_DEFINITION_REPRESENTATION(#9022,#8857);
#8748=PROPERTY_DEFINITION_REPRESENTATION(#9023,#8858);
#8749=PROPERTY_DEFINITION_REPRESENTATION(#9024,#8859);
#8750=PROPERTY_DEFINITION_REPRESENTATION(#9025,#8860);
#8751=PROPERTY_DEFINITION_REPRESENTATION(#9026,#8861);
#8752=PROPERTY_DEFINITION_REPRESENTATION(#9027,#8862);
#8753=PROPERTY_DEFINITION_REPRESENTATION(#9028,#8863);
#8754=PROPERTY_DEFINITION_REPRESENTATION(#9029,#8864);
#8755=PROPERTY_DEFINITION_REPRESENTATION(#9030,#8865);
#8756=PROPERTY_DEFINITION_REPRESENTATION(#9031,#8866);
#8757=PROPERTY_DEFINITION_REPRESENTATION(#9032,#8867);
#8758=PROPERTY_DEFINITION_REPRESENTATION(#9033,#8868);
#8759=PROPERTY_DEFINITION_REPRESENTATION(#9034,#8869);
#8760=PROPERTY_DEFINITION_REPRESENTATION(#9035,#8870);
#8761=PROPERTY_DEFINITION_REPRESENTATION(#9036,#8871);
#8762=PROPERTY_DEFINITION_REPRESENTATION(#9037,#8872);
#8763=PROPERTY_DEFINITION_REPRESENTATION(#9038,#8873);
#8764=PROPERTY_DEFINITION_REPRESENTATION(#9039,#8874);
#8765=REPRESENTATION('material name',(#8875),#16215);
#8766=REPRESENTATION('density',(#8600),#16215);
#8767=REPRESENTATION('material name',(#8876),#16216);
#8768=REPRESENTATION('density',(#8601),#16216);
#8769=REPRESENTATION('material name',(#8877),#16217);
#8770=REPRESENTATION('density',(#8602),#16217);
#8771=REPRESENTATION('material name',(#8878),#16218);
#8772=REPRESENTATION('density',(#8603),#16218);
#8773=REPRESENTATION('material name',(#8879),#16220);
#8774=REPRESENTATION('density',(#8604),#16220);
#8775=REPRESENTATION('material name',(#8880),#16221);
#8776=REPRESENTATION('density',(#8605),#16221);
#8777=REPRESENTATION('material name',(#8881),#16222);
#8778=REPRESENTATION('density',(#8606),#16222);
#8779=REPRESENTATION('material name',(#8882),#16223);
#8780=REPRESENTATION('density',(#8607),#16223);
#8781=REPRESENTATION('material name',(#8883),#16224);
#8782=REPRESENTATION('density',(#8608),#16224);
#8783=REPRESENTATION('material name',(#8884),#16225);
#8784=REPRESENTATION('density',(#8609),#16225);
#8785=REPRESENTATION('material name',(#8885),#16226);
#8786=REPRESENTATION('density',(#8610),#16226);
#8787=REPRESENTATION('material name',(#8886),#16228);
#8788=REPRESENTATION('density',(#8611),#16228);
#8789=REPRESENTATION('material name',(#8887),#16229);
#8790=REPRESENTATION('density',(#8612),#16229);
#8791=REPRESENTATION('material name',(#8888),#16230);
#8792=REPRESENTATION('density',(#8613),#16230);
#8793=REPRESENTATION('material name',(#8889),#16231);
#8794=REPRESENTATION('density',(#8614),#16231);
#8795=REPRESENTATION('material name',(#8890),#16232);
#8796=REPRESENTATION('density',(#8615),#16232);
#8797=REPRESENTATION('material name',(#8891),#16234);
#8798=REPRESENTATION('density',(#8616),#16234);
#8799=REPRESENTATION('material name',(#8892),#16235);
#8800=REPRESENTATION('density',(#8617),#16235);
#8801=REPRESENTATION('material name',(#8893),#16236);
#8802=REPRESENTATION('density',(#8618),#16236);
#8803=REPRESENTATION('material name',(#8894),#16237);
#8804=REPRESENTATION('density',(#8619),#16237);
#8805=REPRESENTATION('material name',(#8895),#16238);
#8806=REPRESENTATION('density',(#8620),#16238);
#8807=REPRESENTATION('material name',(#8896),#16240);
#8808=REPRESENTATION('density',(#8621),#16240);
#8809=REPRESENTATION('material name',(#8897),#16241);
#8810=REPRESENTATION('density',(#8622),#16241);
#8811=REPRESENTATION('material name',(#8898),#16242);
#8812=REPRESENTATION('density',(#8623),#16242);
#8813=REPRESENTATION('material name',(#8899),#16243);
#8814=REPRESENTATION('density',(#8624),#16243);
#8815=REPRESENTATION('material name',(#8900),#16244);
#8816=REPRESENTATION('density',(#8625),#16244);
#8817=REPRESENTATION('material name',(#8901),#16246);
#8818=REPRESENTATION('density',(#8626),#16246);
#8819=REPRESENTATION('material name',(#8902),#16247);
#8820=REPRESENTATION('density',(#8627),#16247);
#8821=REPRESENTATION('material name',(#8903),#16248);
#8822=REPRESENTATION('density',(#8628),#16248);
#8823=REPRESENTATION('material name',(#8904),#16249);
#8824=REPRESENTATION('density',(#8629),#16249);
#8825=REPRESENTATION('material name',(#8905),#16250);
#8826=REPRESENTATION('density',(#8630),#16250);
#8827=REPRESENTATION('material name',(#8906),#16252);
#8828=REPRESENTATION('density',(#8631),#16252);
#8829=REPRESENTATION('material name',(#8907),#16253);
#8830=REPRESENTATION('density',(#8632),#16253);
#8831=REPRESENTATION('material name',(#8908),#16254);
#8832=REPRESENTATION('density',(#8633),#16254);
#8833=REPRESENTATION('material name',(#8909),#16255);
#8834=REPRESENTATION('density',(#8634),#16255);
#8835=REPRESENTATION('material name',(#8910),#16256);
#8836=REPRESENTATION('density',(#8635),#16256);
#8837=REPRESENTATION('material name',(#8911),#16257);
#8838=REPRESENTATION('density',(#8636),#16257);
#8839=REPRESENTATION('material name',(#8912),#16258);
#8840=REPRESENTATION('density',(#8637),#16258);
#8841=REPRESENTATION('material name',(#8913),#16260);
#8842=REPRESENTATION('density',(#8638),#16260);
#8843=REPRESENTATION('material name',(#8914),#16261);
#8844=REPRESENTATION('density',(#8639),#16261);
#8845=REPRESENTATION('material name',(#8915),#16262);
#8846=REPRESENTATION('density',(#8640),#16262);
#8847=REPRESENTATION('material name',(#8916),#16264);
#8848=REPRESENTATION('density',(#8641),#16264);
#8849=REPRESENTATION('material name',(#8917),#16265);
#8850=REPRESENTATION('density',(#8642),#16265);
#8851=REPRESENTATION('material name',(#8918),#16266);
#8852=REPRESENTATION('density',(#8643),#16266);
#8853=REPRESENTATION('material name',(#8919),#16268);
#8854=REPRESENTATION('density',(#8644),#16268);
#8855=REPRESENTATION('material name',(#8920),#16269);
#8856=REPRESENTATION('density',(#8645),#16269);
#8857=REPRESENTATION('material name',(#8921),#16270);
#8858=REPRESENTATION('density',(#8646),#16270);
#8859=REPRESENTATION('material name',(#8922),#16272);
#8860=REPRESENTATION('density',(#8647),#16272);
#8861=REPRESENTATION('material name',(#8923),#16273);
#8862=REPRESENTATION('density',(#8648),#16273);
#8863=REPRESENTATION('material name',(#8924),#16274);
#8864=REPRESENTATION('density',(#8649),#16274);
#8865=REPRESENTATION('material name',(#8925),#16276);
#8866=REPRESENTATION('density',(#8650),#16276);
#8867=REPRESENTATION('material name',(#8926),#16277);
#8868=REPRESENTATION('density',(#8651),#16277);
#8869=REPRESENTATION('material name',(#8927),#16278);
#8870=REPRESENTATION('density',(#8652),#16278);
#8871=REPRESENTATION('material name',(#8928),#16279);
#8872=REPRESENTATION('density',(#8653),#16279);
#8873=REPRESENTATION('material name',(#8929),#16280);
#8874=REPRESENTATION('density',(#8654),#16280);
#8875=DESCRIPTIVE_REPRESENTATION_ITEM('Steel','Steel');
#8876=DESCRIPTIVE_REPRESENTATION_ITEM('Steel','Steel');
#8877=DESCRIPTIVE_REPRESENTATION_ITEM('Steel','Steel');
#8878=DESCRIPTIVE_REPRESENTATION_ITEM('Steel','Steel');
#8879=DESCRIPTIVE_REPRESENTATION_ITEM('Steel','Steel');
#8880=DESCRIPTIVE_REPRESENTATION_ITEM('Steel','Steel');
#8881=DESCRIPTIVE_REPRESENTATION_ITEM('Steel','Steel');
#8882=DESCRIPTIVE_REPRESENTATION_ITEM('Steel','Steel');
#8883=DESCRIPTIVE_REPRESENTATION_ITEM('Steel','Steel');
#8884=DESCRIPTIVE_REPRESENTATION_ITEM('Steel','Steel');
#8885=DESCRIPTIVE_REPRESENTATION_ITEM('Steel','Steel');
#8886=DESCRIPTIVE_REPRESENTATION_ITEM('Steel','Steel');
#8887=DESCRIPTIVE_REPRESENTATION_ITEM('Steel','Steel');
#8888=DESCRIPTIVE_REPRESENTATION_ITEM('Steel','Steel');
#8889=DESCRIPTIVE_REPRESENTATION_ITEM('Steel','Steel');
#8890=DESCRIPTIVE_REPRESENTATION_ITEM('Steel','Steel');
#8891=DESCRIPTIVE_REPRESENTATION_ITEM('Steel','Steel');
#8892=DESCRIPTIVE_REPRESENTATION_ITEM('Steel','Steel');
#8893=DESCRIPTIVE_REPRESENTATION_ITEM('Steel','Steel');
#8894=DESCRIPTIVE_REPRESENTATION_ITEM('Steel','Steel');
#8895=DESCRIPTIVE_REPRESENTATION_ITEM('Steel','Steel');
#8896=DESCRIPTIVE_REPRESENTATION_ITEM('Steel','Steel');
#8897=DESCRIPTIVE_REPRESENTATION_ITEM('Steel','Steel');
#8898=DESCRIPTIVE_REPRESENTATION_ITEM('Steel','Steel');
#8899=DESCRIPTIVE_REPRESENTATION_ITEM('Steel','Steel');
#8900=DESCRIPTIVE_REPRESENTATION_ITEM('Steel','Steel');
#8901=DESCRIPTIVE_REPRESENTATION_ITEM('Steel','Steel');
#8902=DESCRIPTIVE_REPRESENTATION_ITEM('Steel','Steel');
#8903=DESCRIPTIVE_REPRESENTATION_ITEM('Steel','Steel');
#8904=DESCRIPTIVE_REPRESENTATION_ITEM('Steel','Steel');
#8905=DESCRIPTIVE_REPRESENTATION_ITEM('Steel','Steel');
#8906=DESCRIPTIVE_REPRESENTATION_ITEM('Steel','Steel');
#8907=DESCRIPTIVE_REPRESENTATION_ITEM('Steel','Steel');
#8908=DESCRIPTIVE_REPRESENTATION_ITEM('Steel','Steel');
#8909=DESCRIPTIVE_REPRESENTATION_ITEM('Steel','Steel');
#8910=DESCRIPTIVE_REPRESENTATION_ITEM('Steel','Steel');
#8911=DESCRIPTIVE_REPRESENTATION_ITEM('Steel','Steel');
#8912=DESCRIPTIVE_REPRESENTATION_ITEM('Steel','Steel');
#8913=DESCRIPTIVE_REPRESENTATION_ITEM('Steel','Steel');
#8914=DESCRIPTIVE_REPRESENTATION_ITEM('Steel','Steel');
#8915=DESCRIPTIVE_REPRESENTATION_ITEM('Steel','Steel');
#8916=DESCRIPTIVE_REPRESENTATION_ITEM('Steel','Steel');
#8917=DESCRIPTIVE_REPRESENTATION_ITEM('Steel','Steel');
#8918=DESCRIPTIVE_REPRESENTATION_ITEM('Steel','Steel');
#8919=DESCRIPTIVE_REPRESENTATION_ITEM('Steel','Steel');
#8920=DESCRIPTIVE_REPRESENTATION_ITEM('Steel','Steel');
#8921=DESCRIPTIVE_REPRESENTATION_ITEM('Steel','Steel');
#8922=DESCRIPTIVE_REPRESENTATION_ITEM('Steel','Steel');
#8923=DESCRIPTIVE_REPRESENTATION_ITEM('Steel','Steel');
#8924=DESCRIPTIVE_REPRESENTATION_ITEM('Steel','Steel');
#8925=DESCRIPTIVE_REPRESENTATION_ITEM('Steel','Steel');
#8926=DESCRIPTIVE_REPRESENTATION_ITEM('Steel','Steel');
#8927=DESCRIPTIVE_REPRESENTATION_ITEM('Steel','Steel');
#8928=DESCRIPTIVE_REPRESENTATION_ITEM('Steel','Steel');
#8929=DESCRIPTIVE_REPRESENTATION_ITEM('Steel','Steel');
#8930=PROPERTY_DEFINITION('material property','material name',#16590);
#8931=PROPERTY_DEFINITION('material property','density of part',#16590);
#8932=PROPERTY_DEFINITION('material property','material name',#16591);
#8933=PROPERTY_DEFINITION('material property','density of part',#16591);
#8934=PROPERTY_DEFINITION('material property','material name',#16592);
#8935=PROPERTY_DEFINITION('material property','density of part',#16592);
#8936=PROPERTY_DEFINITION('material property','material name',#16593);
#8937=PROPERTY_DEFINITION('material property','density of part',#16593);
#8938=PROPERTY_DEFINITION('material property','material name',#16595);
#8939=PROPERTY_DEFINITION('material property','density of part',#16595);
#8940=PROPERTY_DEFINITION('material property','material name',#16596);
#8941=PROPERTY_DEFINITION('material property','density of part',#16596);
#8942=PROPERTY_DEFINITION('material property','material name',#16597);
#8943=PROPERTY_DEFINITION('material property','density of part',#16597);
#8944=PROPERTY_DEFINITION('material property','material name',#16598);
#8945=PROPERTY_DEFINITION('material property','density of part',#16598);
#8946=PROPERTY_DEFINITION('material property','material name',#16599);
#8947=PROPERTY_DEFINITION('material property','density of part',#16599);
#8948=PROPERTY_DEFINITION('material property','material name',#16600);
#8949=PROPERTY_DEFINITION('material property','density of part',#16600);
#8950=PROPERTY_DEFINITION('material property','material name',#16601);
#8951=PROPERTY_DEFINITION('material property','density of part',#16601);
#8952=PROPERTY_DEFINITION('material property','material name',#16603);
#8953=PROPERTY_DEFINITION('material property','density of part',#16603);
#8954=PROPERTY_DEFINITION('material property','material name',#16604);
#8955=PROPERTY_DEFINITION('material property','density of part',#16604);
#8956=PROPERTY_DEFINITION('material property','material name',#16605);
#8957=PROPERTY_DEFINITION('material property','density of part',#16605);
#8958=PROPERTY_DEFINITION('material property','material name',#16606);
#8959=PROPERTY_DEFINITION('material property','density of part',#16606);
#8960=PROPERTY_DEFINITION('material property','material name',#16607);
#8961=PROPERTY_DEFINITION('material property','density of part',#16607);
#8962=PROPERTY_DEFINITION('material property','material name',#16609);
#8963=PROPERTY_DEFINITION('material property','density of part',#16609);
#8964=PROPERTY_DEFINITION('material property','material name',#16610);
#8965=PROPERTY_DEFINITION('material property','density of part',#16610);
#8966=PROPERTY_DEFINITION('material property','material name',#16611);
#8967=PROPERTY_DEFINITION('material property','density of part',#16611);
#8968=PROPERTY_DEFINITION('material property','material name',#16612);
#8969=PROPERTY_DEFINITION('material property','density of part',#16612);
#8970=PROPERTY_DEFINITION('material property','material name',#16613);
#8971=PROPERTY_DEFINITION('material property','density of part',#16613);
#8972=PROPERTY_DEFINITION('material property','material name',#16615);
#8973=PROPERTY_DEFINITION('material property','density of part',#16615);
#8974=PROPERTY_DEFINITION('material property','material name',#16616);
#8975=PROPERTY_DEFINITION('material property','density of part',#16616);
#8976=PROPERTY_DEFINITION('material property','material name',#16617);
#8977=PROPERTY_DEFINITION('material property','density of part',#16617);
#8978=PROPERTY_DEFINITION('material property','material name',#16618);
#8979=PROPERTY_DEFINITION('material property','density of part',#16618);
#8980=PROPERTY_DEFINITION('material property','material name',#16619);
#8981=PROPERTY_DEFINITION('material property','density of part',#16619);
#8982=PROPERTY_DEFINITION('material property','material name',#16621);
#8983=PROPERTY_DEFINITION('material property','density of part',#16621);
#8984=PROPERTY_DEFINITION('material property','material name',#16622);
#8985=PROPERTY_DEFINITION('material property','density of part',#16622);
#8986=PROPERTY_DEFINITION('material property','material name',#16623);
#8987=PROPERTY_DEFINITION('material property','density of part',#16623);
#8988=PROPERTY_DEFINITION('material property','material name',#16624);
#8989=PROPERTY_DEFINITION('material property','density of part',#16624);
#8990=PROPERTY_DEFINITION('material property','material name',#16625);
#8991=PROPERTY_DEFINITION('material property','density of part',#16625);
#8992=PROPERTY_DEFINITION('material property','material name',#16627);
#8993=PROPERTY_DEFINITION('material property','density of part',#16627);
#8994=PROPERTY_DEFINITION('material property','material name',#16628);
#8995=PROPERTY_DEFINITION('material property','density of part',#16628);
#8996=PROPERTY_DEFINITION('material property','material name',#16629);
#8997=PROPERTY_DEFINITION('material property','density of part',#16629);
#8998=PROPERTY_DEFINITION('material property','material name',#16630);
#8999=PROPERTY_DEFINITION('material property','density of part',#16630);
#9000=PROPERTY_DEFINITION('material property','material name',#16631);
#9001=PROPERTY_DEFINITION('material property','density of part',#16631);
#9002=PROPERTY_DEFINITION('material property','material name',#16632);
#9003=PROPERTY_DEFINITION('material property','density of part',#16632);
#9004=PROPERTY_DEFINITION('material property','material name',#16633);
#9005=PROPERTY_DEFINITION('material property','density of part',#16633);
#9006=PROPERTY_DEFINITION('material property','material name',#16635);
#9007=PROPERTY_DEFINITION('material property','density of part',#16635);
#9008=PROPERTY_DEFINITION('material property','material name',#16636);
#9009=PROPERTY_DEFINITION('material property','density of part',#16636);
#9010=PROPERTY_DEFINITION('material property','material name',#16637);
#9011=PROPERTY_DEFINITION('material property','density of part',#16637);
#9012=PROPERTY_DEFINITION('material property','material name',#16639);
#9013=PROPERTY_DEFINITION('material property','density of part',#16639);
#9014=PROPERTY_DEFINITION('material property','material name',#16640);
#9015=PROPERTY_DEFINITION('material property','density of part',#16640);
#9016=PROPERTY_DEFINITION('material property','material name',#16641);
#9017=PROPERTY_DEFINITION('material property','density of part',#16641);
#9018=PROPERTY_DEFINITION('material property','material name',#16643);
#9019=PROPERTY_DEFINITION('material property','density of part',#16643);
#9020=PROPERTY_DEFINITION('material property','material name',#16644);
#9021=PROPERTY_DEFINITION('material property','density of part',#16644);
#9022=PROPERTY_DEFINITION('material property','material name',#16645);
#9023=PROPERTY_DEFINITION('material property','density of part',#16645);
#9024=PROPERTY_DEFINITION('material property','material name',#16647);
#9025=PROPERTY_DEFINITION('material property','density of part',#16647);
#9026=PROPERTY_DEFINITION('material property','material name',#16648);
#9027=PROPERTY_DEFINITION('material property','density of part',#16648);
#9028=PROPERTY_DEFINITION('material property','material name',#16649);
#9029=PROPERTY_DEFINITION('material property','density of part',#16649);
#9030=PROPERTY_DEFINITION('material property','material name',#16651);
#9031=PROPERTY_DEFINITION('material property','density of part',#16651);
#9032=PROPERTY_DEFINITION('material property','material name',#16652);
#9033=PROPERTY_DEFINITION('material property','density of part',#16652);
#9034=PROPERTY_DEFINITION('material property','material name',#16653);
#9035=PROPERTY_DEFINITION('material property','density of part',#16653);
#9036=PROPERTY_DEFINITION('material property','material name',#16654);
#9037=PROPERTY_DEFINITION('material property','density of part',#16654);
#9038=PROPERTY_DEFINITION('material property','material name',#16655);
#9039=PROPERTY_DEFINITION('material property','density of part',#16655);
#9040=AXIS2_PLACEMENT_3D('',#13003,#10200,#10201);
#9041=AXIS2_PLACEMENT_3D('',#13004,#10202,#10203);
#9042=AXIS2_PLACEMENT_3D('',#13005,#10204,#10205);
#9043=AXIS2_PLACEMENT_3D('',#13006,#10206,#10207);
#9044=AXIS2_PLACEMENT_3D('',#13008,#10208,#10209);
#9045=AXIS2_PLACEMENT_3D('',#13011,#10211,#10212);
#9046=AXIS2_PLACEMENT_3D('',#13012,#10213,#10214);
#9047=AXIS2_PLACEMENT_3D('',#13014,#10215,#10216);
#9048=AXIS2_PLACEMENT_3D('',#13017,#10218,#10219);
#9049=AXIS2_PLACEMENT_3D('',#13018,#10220,#10221);
#9050=AXIS2_PLACEMENT_3D('',#13020,#10222,#10223);
#9051=AXIS2_PLACEMENT_3D('',#13023,#10225,#10226);
#9052=AXIS2_PLACEMENT_3D('',#13024,#10227,#10228);
#9053=AXIS2_PLACEMENT_3D('',#13026,#10229,#10230);
#9054=AXIS2_PLACEMENT_3D('',#13029,#10232,#10233);
#9055=AXIS2_PLACEMENT_3D('',#13030,#10234,#10235);
#9056=AXIS2_PLACEMENT_3D('',#13032,#10236,#10237);
#9057=AXIS2_PLACEMENT_3D('',#13035,#10239,#10240);
#9058=AXIS2_PLACEMENT_3D('',#13036,#10241,#10242);
#9059=AXIS2_PLACEMENT_3D('',#13038,#10243,#10244);
#9060=AXIS2_PLACEMENT_3D('',#13041,#10246,#10247);
#9061=AXIS2_PLACEMENT_3D('',#13042,#10248,#10249);
#9062=AXIS2_PLACEMENT_3D('',#13044,#10250,#10251);
#9063=AXIS2_PLACEMENT_3D('',#13047,#10253,#10254);
#9064=AXIS2_PLACEMENT_3D('',#13048,#10255,#10256);
#9065=AXIS2_PLACEMENT_3D('',#13050,#10257,#10258);
#9066=AXIS2_PLACEMENT_3D('',#13053,#10260,#10261);
#9067=AXIS2_PLACEMENT_3D('',#13054,#10262,#10263);
#9068=AXIS2_PLACEMENT_3D('',#13056,#10264,#10265);
#9069=AXIS2_PLACEMENT_3D('',#13059,#10267,#10268);
#9070=AXIS2_PLACEMENT_3D('',#13060,#10269,#10270);
#9071=AXIS2_PLACEMENT_3D('',#13062,#10271,#10272);
#9072=AXIS2_PLACEMENT_3D('',#13065,#10274,#10275);
#9073=AXIS2_PLACEMENT_3D('',#13066,#10276,#10277);
#9074=AXIS2_PLACEMENT_3D('',#13068,#10278,#10279);
#9075=AXIS2_PLACEMENT_3D('',#13071,#10281,#10282);
#9076=AXIS2_PLACEMENT_3D('',#13072,#10283,#10284);
#9077=AXIS2_PLACEMENT_3D('',#13074,#10285,#10286);
#9078=AXIS2_PLACEMENT_3D('',#13077,#10288,#10289);
#9079=AXIS2_PLACEMENT_3D('',#13078,#10290,#10291);
#9080=AXIS2_PLACEMENT_3D('',#13080,#10292,#10293);
#9081=AXIS2_PLACEMENT_3D('',#13083,#10295,#10296);
#9082=AXIS2_PLACEMENT_3D('',#13084,#10297,#10298);
#9083=AXIS2_PLACEMENT_3D('',#13086,#10299,#10300);
#9084=AXIS2_PLACEMENT_3D('',#13089,#10302,#10303);
#9085=AXIS2_PLACEMENT_3D('',#13090,#10304,#10305);
#9086=AXIS2_PLACEMENT_3D('',#13092,#10306,#10307);
#9087=AXIS2_PLACEMENT_3D('',#13095,#10309,#10310);
#9088=AXIS2_PLACEMENT_3D('',#13096,#10311,#10312);
#9089=AXIS2_PLACEMENT_3D('',#13098,#10313,#10314);
#9090=AXIS2_PLACEMENT_3D('',#13101,#10316,#10317);
#9091=AXIS2_PLACEMENT_3D('',#13102,#10318,#10319);
#9092=AXIS2_PLACEMENT_3D('',#13104,#10320,#10321);
#9093=AXIS2_PLACEMENT_3D('',#13107,#10323,#10324);
#9094=AXIS2_PLACEMENT_3D('',#13108,#10325,#10326);
#9095=AXIS2_PLACEMENT_3D('',#13110,#10327,#10328);
#9096=AXIS2_PLACEMENT_3D('',#13113,#10330,#10331);
#9097=AXIS2_PLACEMENT_3D('',#13114,#10332,#10333);
#9098=AXIS2_PLACEMENT_3D('',#13116,#10334,#10335);
#9099=AXIS2_PLACEMENT_3D('',#13119,#10337,#10338);
#9100=AXIS2_PLACEMENT_3D('',#13120,#10339,#10340);
#9101=AXIS2_PLACEMENT_3D('',#13122,#10341,#10342);
#9102=AXIS2_PLACEMENT_3D('',#13125,#10344,#10345);
#9103=AXIS2_PLACEMENT_3D('',#13126,#10346,#10347);
#9104=AXIS2_PLACEMENT_3D('',#13135,#10352,#10353);
#9105=AXIS2_PLACEMENT_3D('',#13141,#10357,#10358);
#9106=AXIS2_PLACEMENT_3D('',#13147,#10362,#10363);
#9107=AXIS2_PLACEMENT_3D('',#13150,#10366,#10367);
#9108=AXIS2_PLACEMENT_3D('',#13151,#10368,#10369);
#9109=AXIS2_PLACEMENT_3D('',#13152,#10370,#10371);
#9110=AXIS2_PLACEMENT_3D('',#13153,#10372,#10373);
#9111=AXIS2_PLACEMENT_3D('',#13158,#10375,#10376);
#9112=AXIS2_PLACEMENT_3D('',#13161,#10378,#10379);
#9113=AXIS2_PLACEMENT_3D('',#13162,#10380,#10381);
#9114=AXIS2_PLACEMENT_3D('',#13167,#10383,#10384);
#9115=AXIS2_PLACEMENT_3D('',#13170,#10386,#10387);
#9116=AXIS2_PLACEMENT_3D('',#13171,#10388,#10389);
#9117=AXIS2_PLACEMENT_3D('',#13176,#10391,#10392);
#9118=AXIS2_PLACEMENT_3D('',#13179,#10394,#10395);
#9119=AXIS2_PLACEMENT_3D('',#13180,#10396,#10397);
#9120=AXIS2_PLACEMENT_3D('',#13185,#10399,#10400);
#9121=AXIS2_PLACEMENT_3D('',#13188,#10402,#10403);
#9122=AXIS2_PLACEMENT_3D('',#13189,#10404,#10405);
#9123=AXIS2_PLACEMENT_3D('',#13191,#10406,#10407);
#9124=AXIS2_PLACEMENT_3D('',#13194,#10409,#10410);
#9125=AXIS2_PLACEMENT_3D('',#13195,#10411,#10412);
#9126=AXIS2_PLACEMENT_3D('',#13196,#10413,#10414);
#9127=AXIS2_PLACEMENT_3D('',#13198,#10415,#10416);
#9128=AXIS2_PLACEMENT_3D('',#13201,#10418,#10419);
#9129=AXIS2_PLACEMENT_3D('',#13202,#10420,#10421);
#9130=AXIS2_PLACEMENT_3D('',#13203,#10422,#10423);
#9131=AXIS2_PLACEMENT_3D('',#13205,#10424,#10425);
#9132=AXIS2_PLACEMENT_3D('',#13208,#10427,#10428);
#9133=AXIS2_PLACEMENT_3D('',#13209,#10429,#10430);
#9134=AXIS2_PLACEMENT_3D('',#13210,#10431,#10432);
#9135=AXIS2_PLACEMENT_3D('',#13212,#10433,#10434);
#9136=AXIS2_PLACEMENT_3D('',#13215,#10436,#10437);
#9137=AXIS2_PLACEMENT_3D('',#13216,#10438,#10439);
#9138=AXIS2_PLACEMENT_3D('',#13217,#10440,#10441);
#9139=AXIS2_PLACEMENT_3D('',#13218,#10442,#10443);
#9140=AXIS2_PLACEMENT_3D('',#13220,#10445,#10446);
#9141=AXIS2_PLACEMENT_3D('',#13221,#10447,#10448);
#9142=AXIS2_PLACEMENT_3D('',#13223,#10449,#10450);
#9143=AXIS2_PLACEMENT_3D('',#13224,#10451,#10452);
#9144=AXIS2_PLACEMENT_3D('',#13225,#10453,#10454);
#9145=AXIS2_PLACEMENT_3D('',#13227,#10456,#10457);
#9146=AXIS2_PLACEMENT_3D('',#13228,#10458,#10459);
#9147=AXIS2_PLACEMENT_3D('',#13230,#10460,#10461);
#9148=AXIS2_PLACEMENT_3D('',#13231,#10462,#10463);
#9149=AXIS2_PLACEMENT_3D('',#13232,#10464,#10465);
#9150=AXIS2_PLACEMENT_3D('',#13234,#10467,#10468);
#9151=AXIS2_PLACEMENT_3D('',#13235,#10469,#10470);
#9152=AXIS2_PLACEMENT_3D('',#13237,#10471,#10472);
#9153=AXIS2_PLACEMENT_3D('',#13238,#10473,#10474);
#9154=AXIS2_PLACEMENT_3D('',#13239,#10475,#10476);
#9155=AXIS2_PLACEMENT_3D('',#13241,#10478,#10479);
#9156=AXIS2_PLACEMENT_3D('',#13242,#10480,#10481);
#9157=AXIS2_PLACEMENT_3D('',#13244,#10482,#10483);
#9158=AXIS2_PLACEMENT_3D('',#13245,#10484,#10485);
#9159=AXIS2_PLACEMENT_3D('',#13246,#10486,#10487);
#9160=AXIS2_PLACEMENT_3D('',#13247,#10488,#10489);
#9161=AXIS2_PLACEMENT_3D('',#13248,#10490,#10491);
#9162=AXIS2_PLACEMENT_3D('',#13249,#10492,#10493);
#9163=AXIS2_PLACEMENT_3D('',#13251,#10494,#10495);
#9164=AXIS2_PLACEMENT_3D('',#13252,#10496,#10497);
#9165=AXIS2_PLACEMENT_3D('',#13254,#10498,#10499);
#9166=AXIS2_PLACEMENT_3D('',#13256,#10501,#10502);
#9167=AXIS2_PLACEMENT_3D('',#13258,#10503,#10504);
#9168=AXIS2_PLACEMENT_3D('',#13260,#10506,#10507);
#9169=AXIS2_PLACEMENT_3D('',#13262,#10508,#10509);
#9170=AXIS2_PLACEMENT_3D('',#13264,#10511,#10512);
#9171=AXIS2_PLACEMENT_3D('',#13266,#10513,#10514);
#9172=AXIS2_PLACEMENT_3D('',#13268,#10516,#10517);
#9173=AXIS2_PLACEMENT_3D('',#13271,#10519,#10520);
#9174=AXIS2_PLACEMENT_3D('',#13272,#10521,#10522);
#9175=AXIS2_PLACEMENT_3D('',#13274,#10523,#10524);
#9176=AXIS2_PLACEMENT_3D('',#13277,#10526,#10527);
#9177=AXIS2_PLACEMENT_3D('',#13278,#10528,#10529);
#9178=AXIS2_PLACEMENT_3D('',#13281,#10531,#10532);
#9179=AXIS2_PLACEMENT_3D('',#13282,#10533,#10534);
#9180=AXIS2_PLACEMENT_3D('',#13283,#10535,#10536);
#9181=AXIS2_PLACEMENT_3D('',#13284,#10537,#10538);
#9182=AXIS2_PLACEMENT_3D('',#13285,#10539,#10540);
#9183=AXIS2_PLACEMENT_3D('',#13287,#10541,#10542);
#9184=AXIS2_PLACEMENT_3D('',#13290,#10544,#10545);
#9185=AXIS2_PLACEMENT_3D('',#13291,#10546,#10547);
#9186=AXIS2_PLACEMENT_3D('',#13293,#10548,#10549);
#9187=AXIS2_PLACEMENT_3D('',#13296,#10551,#10552);
#9188=AXIS2_PLACEMENT_3D('',#13297,#10553,#10554);
#9189=AXIS2_PLACEMENT_3D('',#13299,#10555,#10556);
#9190=AXIS2_PLACEMENT_3D('',#13302,#10558,#10559);
#9191=AXIS2_PLACEMENT_3D('',#13303,#10560,#10561);
#9192=AXIS2_PLACEMENT_3D('',#13305,#10562,#10563);
#9193=AXIS2_PLACEMENT_3D('',#13308,#10565,#10566);
#9194=AXIS2_PLACEMENT_3D('',#13309,#10567,#10568);
#9195=AXIS2_PLACEMENT_3D('',#13311,#10569,#10570);
#9196=AXIS2_PLACEMENT_3D('',#13314,#10572,#10573);
#9197=AXIS2_PLACEMENT_3D('',#13315,#10574,#10575);
#9198=AXIS2_PLACEMENT_3D('',#13317,#10576,#10577);
#9199=AXIS2_PLACEMENT_3D('',#13318,#10578,#10579);
#9200=AXIS2_PLACEMENT_3D('',#13320,#10580,#10581);
#9201=AXIS2_PLACEMENT_3D('',#13322,#10583,#10584);
#9202=AXIS2_PLACEMENT_3D('',#13324,#10585,#10586);
#9203=AXIS2_PLACEMENT_3D('',#13327,#10588,#10589);
#9204=AXIS2_PLACEMENT_3D('',#13328,#10590,#10591);
#9205=AXIS2_PLACEMENT_3D('',#13329,#10592,#10593);
#9206=AXIS2_PLACEMENT_3D('',#13330,#10594,#10595);
#9207=AXIS2_PLACEMENT_3D('',#13331,#10596,#10597);
#9208=AXIS2_PLACEMENT_3D('',#13340,#10602,#10603);
#9209=AXIS2_PLACEMENT_3D('',#13346,#10607,#10608);
#9210=AXIS2_PLACEMENT_3D('',#13352,#10612,#10613);
#9211=AXIS2_PLACEMENT_3D('',#13358,#10617,#10618);
#9212=AXIS2_PLACEMENT_3D('',#13364,#10622,#10623);
#9213=AXIS2_PLACEMENT_3D('',#13367,#10626,#10627);
#9214=AXIS2_PLACEMENT_3D('',#13368,#10628,#10629);
#9215=AXIS2_PLACEMENT_3D('',#13369,#10630,#10631);
#9216=AXIS2_PLACEMENT_3D('',#13371,#10632,#10633);
#9217=AXIS2_PLACEMENT_3D('',#13372,#10634,#10635);
#9218=AXIS2_PLACEMENT_3D('',#13374,#10636,#10637);
#9219=AXIS2_PLACEMENT_3D('',#13375,#10638,#10639);
#9220=AXIS2_PLACEMENT_3D('',#13377,#10640,#10641);
#9221=AXIS2_PLACEMENT_3D('',#13379,#10643,#10644);
#9222=AXIS2_PLACEMENT_3D('',#13381,#10645,#10646);
#9223=AXIS2_PLACEMENT_3D('',#13383,#10648,#10649);
#9224=AXIS2_PLACEMENT_3D('',#13385,#10650,#10651);
#9225=AXIS2_PLACEMENT_3D('',#13387,#10653,#10654);
#9226=AXIS2_PLACEMENT_3D('',#13389,#10655,#10656);
#9227=AXIS2_PLACEMENT_3D('',#13390,#10657,#10658);
#9228=AXIS2_PLACEMENT_3D('',#13392,#10659,#10660);
#9229=AXIS2_PLACEMENT_3D('',#13394,#10662,#10663);
#9230=AXIS2_PLACEMENT_3D('',#13396,#10665,#10666);
#9231=AXIS2_PLACEMENT_3D('',#13397,#10667,#10668);
#9232=AXIS2_PLACEMENT_3D('',#13398,#10669,#10670);
#9233=AXIS2_PLACEMENT_3D('',#13401,#10671,#10672);
#9234=AXIS2_PLACEMENT_3D('',#13402,#10673,#10674);
#9235=AXIS2_PLACEMENT_3D('',#13404,#10675,#10676);
#9236=AXIS2_PLACEMENT_3D('',#13406,#10677,#10678);
#9237=AXIS2_PLACEMENT_3D('',#13407,#10679,#10680);
#9238=AXIS2_PLACEMENT_3D('',#13408,#10681,#10682);
#9239=AXIS2_PLACEMENT_3D('',#13411,#10684,#10685);
#9240=AXIS2_PLACEMENT_3D('',#13412,#10686,#10687);
#9241=AXIS2_PLACEMENT_3D('',#13414,#10688,#10689);
#9242=AXIS2_PLACEMENT_3D('',#13417,#10691,#10692);
#9243=AXIS2_PLACEMENT_3D('',#13418,#10693,#10694);
#9244=AXIS2_PLACEMENT_3D('',#13421,#10696,#10697);
#9245=AXIS2_PLACEMENT_3D('',#13422,#10698,#10699);
#9246=AXIS2_PLACEMENT_3D('',#13423,#10700,#10701);
#9247=AXIS2_PLACEMENT_3D('',#13425,#10702,#10703);
#9248=AXIS2_PLACEMENT_3D('',#13427,#10705,#10706);
#9249=AXIS2_PLACEMENT_3D('',#13429,#10707,#10708);
#9250=AXIS2_PLACEMENT_3D('',#13430,#10709,#10710);
#9251=AXIS2_PLACEMENT_3D('',#13432,#10712,#10713);
#9252=AXIS2_PLACEMENT_3D('',#13433,#10714,#10715);
#9253=AXIS2_PLACEMENT_3D('',#13436,#10716,#10717);
#9254=AXIS2_PLACEMENT_3D('',#13437,#10718,#10719);
#9255=AXIS2_PLACEMENT_3D('',#13439,#10720,#10721);
#9256=AXIS2_PLACEMENT_3D('',#13441,#10722,#10723);
#9257=AXIS2_PLACEMENT_3D('',#13442,#10724,#10725);
#9258=AXIS2_PLACEMENT_3D('',#13443,#10726,#10727);
#9259=AXIS2_PLACEMENT_3D('',#13445,#10728,#10729);
#9260=AXIS2_PLACEMENT_3D('',#13447,#10731,#10732);
#9261=AXIS2_PLACEMENT_3D('',#13449,#10733,#10734);
#9262=AXIS2_PLACEMENT_3D('',#13451,#10735,#10736);
#9263=AXIS2_PLACEMENT_3D('',#13452,#10737,#10738);
#9264=AXIS2_PLACEMENT_3D('',#13454,#10739,#10740);
#9265=AXIS2_PLACEMENT_3D('',#13456,#10742,#10743);
#9266=AXIS2_PLACEMENT_3D('',#13458,#10744,#10745);
#9267=AXIS2_PLACEMENT_3D('',#13460,#10747,#10748);
#9268=AXIS2_PLACEMENT_3D('',#13462,#10749,#10750);
#9269=AXIS2_PLACEMENT_3D('',#13464,#10752,#10753);
#9270=AXIS2_PLACEMENT_3D('',#13465,#10754,#10755);
#9271=AXIS2_PLACEMENT_3D('',#13467,#10757,#10758);
#9272=AXIS2_PLACEMENT_3D('',#13468,#10759,#10760);
#9273=AXIS2_PLACEMENT_3D('',#13471,#10761,#10762);
#9274=AXIS2_PLACEMENT_3D('',#13472,#10763,#10764);
#9275=AXIS2_PLACEMENT_3D('',#13475,#10765,#10766);
#9276=AXIS2_PLACEMENT_3D('',#13476,#10767,#10768);
#9277=AXIS2_PLACEMENT_3D('',#13479,#10769,#10770);
#9278=AXIS2_PLACEMENT_3D('',#13480,#10771,#10772);
#9279=AXIS2_PLACEMENT_3D('',#13483,#10773,#10774);
#9280=AXIS2_PLACEMENT_3D('',#13484,#10775,#10776);
#9281=AXIS2_PLACEMENT_3D('',#13487,#10777,#10778);
#9282=AXIS2_PLACEMENT_3D('',#13488,#10779,#10780);
#9283=AXIS2_PLACEMENT_3D('',#13491,#10781,#10782);
#9284=AXIS2_PLACEMENT_3D('',#13492,#10783,#10784);
#9285=AXIS2_PLACEMENT_3D('',#13495,#10785,#10786);
#9286=AXIS2_PLACEMENT_3D('',#13496,#10787,#10788);
#9287=AXIS2_PLACEMENT_3D('',#13499,#10789,#10790);
#9288=AXIS2_PLACEMENT_3D('',#13500,#10791,#10792);
#9289=AXIS2_PLACEMENT_3D('',#13503,#10793,#10794);
#9290=AXIS2_PLACEMENT_3D('',#13504,#10795,#10796);
#9291=AXIS2_PLACEMENT_3D('',#13505,#10797,#10798);
#9292=AXIS2_PLACEMENT_3D('',#13531,#10799,#10800);
#9293=AXIS2_PLACEMENT_3D('',#13555,#10801,#10802);
#9294=AXIS2_PLACEMENT_3D('',#13556,#10803,#10804);
#9295=AXIS2_PLACEMENT_3D('',#13558,#10805,#10806);
#9296=AXIS2_PLACEMENT_3D('',#13583,#10807,#10808);
#9297=AXIS2_PLACEMENT_3D('',#13608,#10809,#10810);
#9298=AXIS2_PLACEMENT_3D('',#13633,#10811,#10812);
#9299=AXIS2_PLACEMENT_3D('',#13636,#10814,#10815);
#9300=AXIS2_PLACEMENT_3D('',#13638,#10816,#10817);
#9301=AXIS2_PLACEMENT_3D('',#13663,#10818,#10819);
#9302=AXIS2_PLACEMENT_3D('',#13688,#10820,#10821);
#9303=AXIS2_PLACEMENT_3D('',#13713,#10822,#10823);
#9304=AXIS2_PLACEMENT_3D('',#13738,#10824,#10825);
#9305=AXIS2_PLACEMENT_3D('',#13762,#10826,#10827);
#9306=AXIS2_PLACEMENT_3D('',#13763,#10828,#10829);
#9307=AXIS2_PLACEMENT_3D('',#13765,#10830,#10831);
#9308=AXIS2_PLACEMENT_3D('',#13766,#10832,#10833);
#9309=AXIS2_PLACEMENT_3D('',#13767,#10834,#10835);
#9310=AXIS2_PLACEMENT_3D('',#13791,#10836,#10837);
#9311=AXIS2_PLACEMENT_3D('',#13792,#10838,#10839);
#9312=AXIS2_PLACEMENT_3D('',#13794,#10840,#10841);
#9313=AXIS2_PLACEMENT_3D('',#13795,#10842,#10843);
#9314=AXIS2_PLACEMENT_3D('',#13796,#10844,#10845);
#9315=AXIS2_PLACEMENT_3D('',#13820,#10846,#10847);
#9316=AXIS2_PLACEMENT_3D('',#13821,#10848,#10849);
#9317=AXIS2_PLACEMENT_3D('',#13823,#10850,#10851);
#9318=AXIS2_PLACEMENT_3D('',#13824,#10852,#10853);
#9319=AXIS2_PLACEMENT_3D('',#13825,#10854,#10855);
#9320=AXIS2_PLACEMENT_3D('',#13849,#10856,#10857);
#9321=AXIS2_PLACEMENT_3D('',#13850,#10858,#10859);
#9322=AXIS2_PLACEMENT_3D('',#13852,#10860,#10861);
#9323=AXIS2_PLACEMENT_3D('',#13854,#10862,#10863);
#9324=AXIS2_PLACEMENT_3D('',#13855,#10864,#10865);
#9325=AXIS2_PLACEMENT_3D('',#13856,#10866,#10867);
#9326=AXIS2_PLACEMENT_3D('',#13880,#10868,#10869);
#9327=AXIS2_PLACEMENT_3D('',#13881,#10870,#10871);
#9328=AXIS2_PLACEMENT_3D('',#13883,#10872,#10873);
#9329=AXIS2_PLACEMENT_3D('',#13884,#10874,#10875);
#9330=AXIS2_PLACEMENT_3D('',#13885,#10876,#10877);
#9331=AXIS2_PLACEMENT_3D('',#13909,#10878,#10879);
#9332=AXIS2_PLACEMENT_3D('',#13910,#10880,#10881);
#9333=AXIS2_PLACEMENT_3D('',#13912,#10882,#10883);
#9334=AXIS2_PLACEMENT_3D('',#13913,#10884,#10885);
#9335=AXIS2_PLACEMENT_3D('',#13914,#10886,#10887);
#9336=AXIS2_PLACEMENT_3D('',#13938,#10888,#10889);
#9337=AXIS2_PLACEMENT_3D('',#13939,#10890,#10891);
#9338=AXIS2_PLACEMENT_3D('',#13941,#10892,#10893);
#9339=AXIS2_PLACEMENT_3D('',#13942,#10894,#10895);
#9340=AXIS2_PLACEMENT_3D('',#13943,#10896,#10897);
#9341=AXIS2_PLACEMENT_3D('',#13967,#10898,#10899);
#9342=AXIS2_PLACEMENT_3D('',#13968,#10900,#10901);
#9343=AXIS2_PLACEMENT_3D('',#13970,#10902,#10903);
#9344=AXIS2_PLACEMENT_3D('',#13973,#10905,#10906);
#9345=AXIS2_PLACEMENT_3D('',#13997,#10907,#10908);
#9346=AXIS2_PLACEMENT_3D('',#13998,#10909,#10910);
#9347=AXIS2_PLACEMENT_3D('',#13999,#10911,#10912);
#9348=AXIS2_PLACEMENT_3D('',#14000,#10913,#10914);
#9349=AXIS2_PLACEMENT_3D('',#14001,#10915,#10916);
#9350=AXIS2_PLACEMENT_3D('',#14002,#10917,#10918);
#9351=AXIS2_PLACEMENT_3D('',#14003,#10919,#10920);
#9352=AXIS2_PLACEMENT_3D('',#14004,#10921,#10922);
#9353=AXIS2_PLACEMENT_3D('',#14005,#10923,#10924);
#9354=AXIS2_PLACEMENT_3D('',#14007,#10925,#10926);
#9355=AXIS2_PLACEMENT_3D('',#14009,#10927,#10928);
#9356=AXIS2_PLACEMENT_3D('',#14010,#10929,#10930);
#9357=AXIS2_PLACEMENT_3D('',#14012,#10931,#10932);
#9358=AXIS2_PLACEMENT_3D('',#14014,#10934,#10935);
#9359=AXIS2_PLACEMENT_3D('',#14016,#10936,#10937);
#9360=AXIS2_PLACEMENT_3D('',#14017,#10938,#10939);
#9361=AXIS2_PLACEMENT_3D('',#14019,#10941,#10942);
#9362=AXIS2_PLACEMENT_3D('',#14021,#10943,#10944);
#9363=AXIS2_PLACEMENT_3D('',#14023,#10945,#10946);
#9364=AXIS2_PLACEMENT_3D('',#14024,#10947,#10948);
#9365=AXIS2_PLACEMENT_3D('',#14026,#10949,#10950);
#9366=AXIS2_PLACEMENT_3D('',#14028,#10952,#10953);
#9367=AXIS2_PLACEMENT_3D('',#14030,#10954,#10955);
#9368=AXIS2_PLACEMENT_3D('',#14031,#10956,#10957);
#9369=AXIS2_PLACEMENT_3D('',#14033,#10959,#10960);
#9370=AXIS2_PLACEMENT_3D('',#14034,#10961,#10962);
#9371=AXIS2_PLACEMENT_3D('',#14035,#10963,#10964);
#9372=AXIS2_PLACEMENT_3D('',#14036,#10965,#10966);
#9373=AXIS2_PLACEMENT_3D('',#14037,#10967,#10968);
#9374=AXIS2_PLACEMENT_3D('',#14038,#10969,#10970);
#9375=AXIS2_PLACEMENT_3D('',#14039,#10971,#10972);
#9376=AXIS2_PLACEMENT_3D('',#14048,#10977,#10978);
#9377=AXIS2_PLACEMENT_3D('',#14054,#10982,#10983);
#9378=AXIS2_PLACEMENT_3D('',#14060,#10987,#10988);
#9379=AXIS2_PLACEMENT_3D('',#14063,#10991,#10992);
#9380=AXIS2_PLACEMENT_3D('',#14064,#10993,#10994);
#9381=AXIS2_PLACEMENT_3D('',#14065,#10995,#10996);
#9382=AXIS2_PLACEMENT_3D('',#14066,#10997,#10998);
#9383=AXIS2_PLACEMENT_3D('',#14075,#11003,#11004);
#9384=AXIS2_PLACEMENT_3D('',#14081,#11008,#11009);
#9385=AXIS2_PLACEMENT_3D('',#14087,#11013,#11014);
#9386=AXIS2_PLACEMENT_3D('',#14090,#11017,#11018);
#9387=AXIS2_PLACEMENT_3D('',#14091,#11019,#11020);
#9388=AXIS2_PLACEMENT_3D('',#14092,#11021,#11022);
#9389=AXIS2_PLACEMENT_3D('',#14093,#11023,#11024);
#9390=AXIS2_PLACEMENT_3D('',#14094,#11025,#11026);
#9391=AXIS2_PLACEMENT_3D('',#14096,#11027,#11028);
#9392=AXIS2_PLACEMENT_3D('',#14099,#11030,#11031);
#9393=AXIS2_PLACEMENT_3D('',#14100,#11032,#11033);
#9394=AXIS2_PLACEMENT_3D('',#14101,#11034,#11035);
#9395=AXIS2_PLACEMENT_3D('',#14103,#11036,#11037);
#9396=AXIS2_PLACEMENT_3D('',#14106,#11039,#11040);
#9397=AXIS2_PLACEMENT_3D('',#14107,#11041,#11042);
#9398=AXIS2_PLACEMENT_3D('',#14108,#11043,#11044);
#9399=AXIS2_PLACEMENT_3D('',#14110,#11045,#11046);
#9400=AXIS2_PLACEMENT_3D('',#14113,#11048,#11049);
#9401=AXIS2_PLACEMENT_3D('',#14114,#11050,#11051);
#9402=AXIS2_PLACEMENT_3D('',#14115,#11052,#11053);
#9403=AXIS2_PLACEMENT_3D('',#14117,#11054,#11055);
#9404=AXIS2_PLACEMENT_3D('',#14119,#11056,#11057);
#9405=AXIS2_PLACEMENT_3D('',#14120,#11058,#11059);
#9406=AXIS2_PLACEMENT_3D('',#14122,#11060,#11061);
#9407=AXIS2_PLACEMENT_3D('',#14124,#11063,#11064);
#9408=AXIS2_PLACEMENT_3D('',#14127,#11066,#11067);
#9409=AXIS2_PLACEMENT_3D('',#14128,#11068,#11069);
#9410=AXIS2_PLACEMENT_3D('',#14129,#11070,#11071);
#9411=AXIS2_PLACEMENT_3D('',#14130,#11072,#11073);
#9412=AXIS2_PLACEMENT_3D('',#14131,#11074,#11075);
#9413=AXIS2_PLACEMENT_3D('',#14133,#11076,#11077);
#9414=AXIS2_PLACEMENT_3D('',#14136,#11079,#11080);
#9415=AXIS2_PLACEMENT_3D('',#14137,#11081,#11082);
#9416=AXIS2_PLACEMENT_3D('',#14139,#11083,#11084);
#9417=AXIS2_PLACEMENT_3D('',#14142,#11086,#11087);
#9418=AXIS2_PLACEMENT_3D('',#14143,#11088,#11089);
#9419=AXIS2_PLACEMENT_3D('',#14145,#11090,#11091);
#9420=AXIS2_PLACEMENT_3D('',#14148,#11093,#11094);
#9421=AXIS2_PLACEMENT_3D('',#14149,#11095,#11096);
#9422=AXIS2_PLACEMENT_3D('',#14151,#11097,#11098);
#9423=AXIS2_PLACEMENT_3D('',#14154,#11100,#11101);
#9424=AXIS2_PLACEMENT_3D('',#14155,#11102,#11103);
#9425=AXIS2_PLACEMENT_3D('',#14157,#11104,#11105);
#9426=AXIS2_PLACEMENT_3D('',#14160,#11107,#11108);
#9427=AXIS2_PLACEMENT_3D('',#14161,#11109,#11110);
#9428=AXIS2_PLACEMENT_3D('',#14163,#11111,#11112);
#9429=AXIS2_PLACEMENT_3D('',#14166,#11114,#11115);
#9430=AXIS2_PLACEMENT_3D('',#14167,#11116,#11117);
#9431=AXIS2_PLACEMENT_3D('',#14169,#11118,#11119);
#9432=AXIS2_PLACEMENT_3D('',#14172,#11121,#11122);
#9433=AXIS2_PLACEMENT_3D('',#14173,#11123,#11124);
#9434=AXIS2_PLACEMENT_3D('',#14175,#11125,#11126);
#9435=AXIS2_PLACEMENT_3D('',#14178,#11128,#11129);
#9436=AXIS2_PLACEMENT_3D('',#14179,#11130,#11131);
#9437=AXIS2_PLACEMENT_3D('',#14181,#11132,#11133);
#9438=AXIS2_PLACEMENT_3D('',#14184,#11135,#11136);
#9439=AXIS2_PLACEMENT_3D('',#14185,#11137,#11138);
#9440=AXIS2_PLACEMENT_3D('',#14187,#11139,#11140);
#9441=AXIS2_PLACEMENT_3D('',#14190,#11142,#11143);
#9442=AXIS2_PLACEMENT_3D('',#14191,#11144,#11145);
#9443=AXIS2_PLACEMENT_3D('',#14193,#11146,#11147);
#9444=AXIS2_PLACEMENT_3D('',#14196,#11149,#11150);
#9445=AXIS2_PLACEMENT_3D('',#14197,#11151,#11152);
#9446=AXIS2_PLACEMENT_3D('',#14199,#11153,#11154);
#9447=AXIS2_PLACEMENT_3D('',#14202,#11156,#11157);
#9448=AXIS2_PLACEMENT_3D('',#14203,#11158,#11159);
#9449=AXIS2_PLACEMENT_3D('',#14205,#11160,#11161);
#9450=AXIS2_PLACEMENT_3D('',#14208,#11163,#11164);
#9451=AXIS2_PLACEMENT_3D('',#14209,#11165,#11166);
#9452=AXIS2_PLACEMENT_3D('',#14210,#11167,#11168);
#9453=AXIS2_PLACEMENT_3D('',#14211,#11169,#11170);
#9454=AXIS2_PLACEMENT_3D('',#14212,#11171,#11172);
#9455=AXIS2_PLACEMENT_3D('',#14217,#11174,#11175);
#9456=AXIS2_PLACEMENT_3D('',#14218,#11176,#11177);
#9457=AXIS2_PLACEMENT_3D('',#14219,#11178,#11179);
#9458=AXIS2_PLACEMENT_3D('',#14236,#11180,#11181);
#9459=AXIS2_PLACEMENT_3D('',#14287,#11183,#11184);
#9460=AXIS2_PLACEMENT_3D('',#14289,#11186,#11187);
#9461=AXIS2_PLACEMENT_3D('',#14291,#11188,#11189);
#9462=AXIS2_PLACEMENT_3D('',#14294,#11191,#11192);
#9463=AXIS2_PLACEMENT_3D('',#14295,#11193,#11194);
#9464=AXIS2_PLACEMENT_3D('',#14297,#11195,#11196);
#9465=AXIS2_PLACEMENT_3D('',#14300,#11198,#11199);
#9466=AXIS2_PLACEMENT_3D('',#14301,#11200,#11201);
#9467=AXIS2_PLACEMENT_3D('',#14302,#11202,#11203);
#9468=AXIS2_PLACEMENT_3D('',#14303,#11204,#11205);
#9469=AXIS2_PLACEMENT_3D('',#14304,#11206,#11207);
#9470=AXIS2_PLACEMENT_3D('',#14306,#11208,#11209);
#9471=AXIS2_PLACEMENT_3D('',#14307,#11210,#11211);
#9472=AXIS2_PLACEMENT_3D('',#14309,#11212,#11213);
#9473=AXIS2_PLACEMENT_3D('',#14311,#11215,#11216);
#9474=AXIS2_PLACEMENT_3D('',#14313,#11217,#11218);
#9475=AXIS2_PLACEMENT_3D('',#14315,#11220,#11221);
#9476=AXIS2_PLACEMENT_3D('',#14317,#11222,#11223);
#9477=AXIS2_PLACEMENT_3D('',#14319,#11225,#11226);
#9478=AXIS2_PLACEMENT_3D('',#14321,#11227,#11228);
#9479=AXIS2_PLACEMENT_3D('',#14322,#11229,#11230);
#9480=AXIS2_PLACEMENT_3D('',#14324,#11231,#11232);
#9481=AXIS2_PLACEMENT_3D('',#14326,#11234,#11235);
#9482=AXIS2_PLACEMENT_3D('',#14328,#11236,#11237);
#9483=AXIS2_PLACEMENT_3D('',#14330,#11239,#11240);
#9484=AXIS2_PLACEMENT_3D('',#14332,#11241,#11242);
#9485=AXIS2_PLACEMENT_3D('',#14334,#11244,#11245);
#9486=AXIS2_PLACEMENT_3D('',#14335,#11246,#11247);
#9487=AXIS2_PLACEMENT_3D('',#14344,#11252,#11253);
#9488=AXIS2_PLACEMENT_3D('',#14350,#11257,#11258);
#9489=AXIS2_PLACEMENT_3D('',#14356,#11262,#11263);
#9490=AXIS2_PLACEMENT_3D('',#14362,#11267,#11268);
#9491=AXIS2_PLACEMENT_3D('',#14368,#11272,#11273);
#9492=AXIS2_PLACEMENT_3D('',#14371,#11276,#11277);
#9493=AXIS2_PLACEMENT_3D('',#14372,#11278,#11279);
#9494=AXIS2_PLACEMENT_3D('',#14373,#11280,#11281);
#9495=AXIS2_PLACEMENT_3D('',#14374,#11282,#11283);
#9496=AXIS2_PLACEMENT_3D('',#14375,#11284,#11285);
#9497=AXIS2_PLACEMENT_3D('',#14376,#11286,#11287);
#9498=AXIS2_PLACEMENT_3D('',#14377,#11288,#11289);
#9499=AXIS2_PLACEMENT_3D('',#14378,#11290,#11291);
#9500=AXIS2_PLACEMENT_3D('',#14379,#11292,#11293);
#9501=AXIS2_PLACEMENT_3D('',#14380,#11294,#11295);
#9502=AXIS2_PLACEMENT_3D('',#14381,#11296,#11297);
#9503=AXIS2_PLACEMENT_3D('',#14382,#11298,#11299);
#9504=AXIS2_PLACEMENT_3D('',#14383,#11300,#11301);
#9505=AXIS2_PLACEMENT_3D('',#14384,#11302,#11303);
#9506=AXIS2_PLACEMENT_3D('',#14385,#11304,#11305);
#9507=AXIS2_PLACEMENT_3D('',#14386,#11306,#11307);
#9508=AXIS2_PLACEMENT_3D('',#14387,#11308,#11309);
#9509=AXIS2_PLACEMENT_3D('',#14388,#11310,#11311);
#9510=AXIS2_PLACEMENT_3D('',#14397,#11316,#11317);
#9511=AXIS2_PLACEMENT_3D('',#14403,#11321,#11322);
#9512=AXIS2_PLACEMENT_3D('',#14409,#11326,#11327);
#9513=AXIS2_PLACEMENT_3D('',#14415,#11331,#11332);
#9514=AXIS2_PLACEMENT_3D('',#14421,#11336,#11337);
#9515=AXIS2_PLACEMENT_3D('',#14424,#11340,#11341);
#9516=AXIS2_PLACEMENT_3D('',#14425,#11342,#11343);
#9517=AXIS2_PLACEMENT_3D('',#14427,#11344,#11345);
#9518=AXIS2_PLACEMENT_3D('',#14428,#11346,#11347);
#9519=AXIS2_PLACEMENT_3D('',#14430,#11348,#11349);
#9520=AXIS2_PLACEMENT_3D('',#14432,#11351,#11352);
#9521=AXIS2_PLACEMENT_3D('',#14434,#11353,#11354);
#9522=AXIS2_PLACEMENT_3D('',#14436,#11356,#11357);
#9523=AXIS2_PLACEMENT_3D('',#14438,#11358,#11359);
#9524=AXIS2_PLACEMENT_3D('',#14440,#11361,#11362);
#9525=AXIS2_PLACEMENT_3D('',#14441,#11363,#11364);
#9526=AXIS2_PLACEMENT_3D('',#14442,#11365,#11366);
#9527=AXIS2_PLACEMENT_3D('',#14443,#11367,#11368);
#9528=AXIS2_PLACEMENT_3D('',#14444,#11369,#11370);
#9529=AXIS2_PLACEMENT_3D('',#14445,#11371,#11372);
#9530=AXIS2_PLACEMENT_3D('',#14446,#11373,#11374);
#9531=AXIS2_PLACEMENT_3D('',#14447,#11375,#11376);
#9532=AXIS2_PLACEMENT_3D('',#14448,#11377,#11378);
#9533=AXIS2_PLACEMENT_3D('',#14449,#11379,#11380);
#9534=AXIS2_PLACEMENT_3D('',#14450,#11381,#11382);
#9535=AXIS2_PLACEMENT_3D('',#14452,#11383,#11384);
#9536=AXIS2_PLACEMENT_3D('',#14455,#11386,#11387);
#9537=AXIS2_PLACEMENT_3D('',#14456,#11388,#11389);
#9538=AXIS2_PLACEMENT_3D('',#14458,#11390,#11391);
#9539=AXIS2_PLACEMENT_3D('',#14461,#11393,#11394);
#9540=AXIS2_PLACEMENT_3D('',#14462,#11395,#11396);
#9541=AXIS2_PLACEMENT_3D('',#14464,#11397,#11398);
#9542=AXIS2_PLACEMENT_3D('',#14467,#11400,#11401);
#9543=AXIS2_PLACEMENT_3D('',#14468,#11402,#11403);
#9544=AXIS2_PLACEMENT_3D('',#14470,#11404,#11405);
#9545=AXIS2_PLACEMENT_3D('',#14473,#11407,#11408);
#9546=AXIS2_PLACEMENT_3D('',#14474,#11409,#11410);
#9547=AXIS2_PLACEMENT_3D('',#14476,#11411,#11412);
#9548=AXIS2_PLACEMENT_3D('',#14479,#11414,#11415);
#9549=AXIS2_PLACEMENT_3D('',#14480,#11416,#11417);
#9550=AXIS2_PLACEMENT_3D('',#14482,#11418,#11419);
#9551=AXIS2_PLACEMENT_3D('',#14485,#11421,#11422);
#9552=AXIS2_PLACEMENT_3D('',#14486,#11423,#11424);
#9553=AXIS2_PLACEMENT_3D('',#14495,#11429,#11430);
#9554=AXIS2_PLACEMENT_3D('',#14504,#11435,#11436);
#9555=AXIS2_PLACEMENT_3D('',#14507,#11439,#11440);
#9556=AXIS2_PLACEMENT_3D('',#14509,#11442,#11443);
#9557=AXIS2_PLACEMENT_3D('',#14511,#11445,#11446);
#9558=AXIS2_PLACEMENT_3D('',#14520,#11451,#11452);
#9559=AXIS2_PLACEMENT_3D('',#14529,#11457,#11458);
#9560=AXIS2_PLACEMENT_3D('',#14532,#11461,#11462);
#9561=AXIS2_PLACEMENT_3D('',#14534,#11464,#11465);
#9562=AXIS2_PLACEMENT_3D('',#14536,#11467,#11468);
#9563=AXIS2_PLACEMENT_3D('',#14545,#11473,#11474);
#9564=AXIS2_PLACEMENT_3D('',#14551,#11478,#11479);
#9565=AXIS2_PLACEMENT_3D('',#14557,#11483,#11484);
#9566=AXIS2_PLACEMENT_3D('',#14560,#11487,#11488);
#9567=AXIS2_PLACEMENT_3D('',#14561,#11489,#11490);
#9568=AXIS2_PLACEMENT_3D('',#14562,#11491,#11492);
#9569=AXIS2_PLACEMENT_3D('',#14563,#11493,#11494);
#9570=AXIS2_PLACEMENT_3D('',#14565,#11495,#11496);
#9571=AXIS2_PLACEMENT_3D('',#14568,#11498,#11499);
#9572=AXIS2_PLACEMENT_3D('',#14569,#11500,#11501);
#9573=AXIS2_PLACEMENT_3D('',#14570,#11502,#11503);
#9574=AXIS2_PLACEMENT_3D('',#14572,#11504,#11505);
#9575=AXIS2_PLACEMENT_3D('',#14574,#11506,#11507);
#9576=AXIS2_PLACEMENT_3D('',#14575,#11508,#11509);
#9577=AXIS2_PLACEMENT_3D('',#14578,#11511,#11512);
#9578=AXIS2_PLACEMENT_3D('',#14579,#11513,#11514);
#9579=AXIS2_PLACEMENT_3D('',#14580,#11515,#11516);
#9580=AXIS2_PLACEMENT_3D('',#14582,#11517,#11518);
#9581=AXIS2_PLACEMENT_3D('',#14584,#11520,#11521);
#9582=AXIS2_PLACEMENT_3D('',#14585,#11522,#11523);
#9583=AXIS2_PLACEMENT_3D('',#14586,#11524,#11525);
#9584=AXIS2_PLACEMENT_3D('',#14588,#11526,#11527);
#9585=AXIS2_PLACEMENT_3D('',#14591,#11529,#11530);
#9586=AXIS2_PLACEMENT_3D('',#14592,#11531,#11532);
#9587=AXIS2_PLACEMENT_3D('',#14594,#11533,#11534);
#9588=AXIS2_PLACEMENT_3D('',#14597,#11536,#11537);
#9589=AXIS2_PLACEMENT_3D('',#14598,#11538,#11539);
#9590=AXIS2_PLACEMENT_3D('',#14599,#11540,#11541);
#9591=AXIS2_PLACEMENT_3D('',#14600,#11542,#11543);
#9592=AXIS2_PLACEMENT_3D('',#14601,#11544,#11545);
#9593=AXIS2_PLACEMENT_3D('',#14603,#11546,#11547);
#9594=AXIS2_PLACEMENT_3D('',#14606,#11549,#11550);
#9595=AXIS2_PLACEMENT_3D('',#14607,#11551,#11552);
#9596=AXIS2_PLACEMENT_3D('',#14609,#11553,#11554);
#9597=AXIS2_PLACEMENT_3D('',#14612,#11556,#11557);
#9598=AXIS2_PLACEMENT_3D('',#14613,#11558,#11559);
#9599=AXIS2_PLACEMENT_3D('',#14614,#11560,#11561);
#9600=AXIS2_PLACEMENT_3D('',#14615,#11562,#11563);
#9601=AXIS2_PLACEMENT_3D('',#14616,#11564,#11565);
#9602=AXIS2_PLACEMENT_3D('',#14618,#11566,#11567);
#9603=AXIS2_PLACEMENT_3D('',#14621,#11569,#11570);
#9604=AXIS2_PLACEMENT_3D('',#14622,#11571,#11572);
#9605=AXIS2_PLACEMENT_3D('',#14624,#11573,#11574);
#9606=AXIS2_PLACEMENT_3D('',#14627,#11576,#11577);
#9607=AXIS2_PLACEMENT_3D('',#14628,#11578,#11579);
#9608=AXIS2_PLACEMENT_3D('',#14629,#11580,#11581);
#9609=AXIS2_PLACEMENT_3D('',#14630,#11582,#11583);
#9610=AXIS2_PLACEMENT_3D('',#14631,#11584,#11585);
#9611=AXIS2_PLACEMENT_3D('',#14632,#11586,#11587);
#9612=AXIS2_PLACEMENT_3D('',#14634,#11588,#11589);
#9613=AXIS2_PLACEMENT_3D('',#14637,#11591,#11592);
#9614=AXIS2_PLACEMENT_3D('',#14638,#11593,#11594);
#9615=AXIS2_PLACEMENT_3D('',#14640,#11595,#11596);
#9616=AXIS2_PLACEMENT_3D('',#14643,#11598,#11599);
#9617=AXIS2_PLACEMENT_3D('',#14644,#11600,#11601);
#9618=AXIS2_PLACEMENT_3D('',#14646,#11602,#11603);
#9619=AXIS2_PLACEMENT_3D('',#14649,#11605,#11606);
#9620=AXIS2_PLACEMENT_3D('',#14650,#11607,#11608);
#9621=AXIS2_PLACEMENT_3D('',#14652,#11609,#11610);
#9622=AXIS2_PLACEMENT_3D('',#14655,#11612,#11613);
#9623=AXIS2_PLACEMENT_3D('',#14656,#11614,#11615);
#9624=AXIS2_PLACEMENT_3D('',#14658,#11616,#11617);
#9625=AXIS2_PLACEMENT_3D('',#14661,#11619,#11620);
#9626=AXIS2_PLACEMENT_3D('',#14662,#11621,#11622);
#9627=AXIS2_PLACEMENT_3D('',#14664,#11623,#11624);
#9628=AXIS2_PLACEMENT_3D('',#14667,#11626,#11627);
#9629=AXIS2_PLACEMENT_3D('',#14668,#11628,#11629);
#9630=AXIS2_PLACEMENT_3D('',#14677,#11634,#11635);
#9631=AXIS2_PLACEMENT_3D('',#14686,#11640,#11641);
#9632=AXIS2_PLACEMENT_3D('',#14689,#11644,#11645);
#9633=AXIS2_PLACEMENT_3D('',#14691,#11647,#11648);
#9634=AXIS2_PLACEMENT_3D('',#14693,#11650,#11651);
#9635=AXIS2_PLACEMENT_3D('',#14702,#11656,#11657);
#9636=AXIS2_PLACEMENT_3D('',#14711,#11662,#11663);
#9637=AXIS2_PLACEMENT_3D('',#14714,#11666,#11667);
#9638=AXIS2_PLACEMENT_3D('',#14716,#11669,#11670);
#9639=AXIS2_PLACEMENT_3D('',#14718,#11672,#11673);
#9640=AXIS2_PLACEMENT_3D('',#14727,#11678,#11679);
#9641=AXIS2_PLACEMENT_3D('',#14733,#11683,#11684);
#9642=AXIS2_PLACEMENT_3D('',#14739,#11688,#11689);
#9643=AXIS2_PLACEMENT_3D('',#14742,#11692,#11693);
#9644=AXIS2_PLACEMENT_3D('',#14743,#11694,#11695);
#9645=AXIS2_PLACEMENT_3D('',#14744,#11696,#11697);
#9646=AXIS2_PLACEMENT_3D('',#14745,#11698,#11699);
#9647=AXIS2_PLACEMENT_3D('',#14747,#11700,#11701);
#9648=AXIS2_PLACEMENT_3D('',#14750,#11703,#11704);
#9649=AXIS2_PLACEMENT_3D('',#14751,#11705,#11706);
#9650=AXIS2_PLACEMENT_3D('',#14752,#11707,#11708);
#9651=AXIS2_PLACEMENT_3D('',#14754,#11709,#11710);
#9652=AXIS2_PLACEMENT_3D('',#14756,#11711,#11712);
#9653=AXIS2_PLACEMENT_3D('',#14757,#11713,#11714);
#9654=AXIS2_PLACEMENT_3D('',#14760,#11716,#11717);
#9655=AXIS2_PLACEMENT_3D('',#14761,#11718,#11719);
#9656=AXIS2_PLACEMENT_3D('',#14762,#11720,#11721);
#9657=AXIS2_PLACEMENT_3D('',#14764,#11722,#11723);
#9658=AXIS2_PLACEMENT_3D('',#14766,#11725,#11726);
#9659=AXIS2_PLACEMENT_3D('',#14767,#11727,#11728);
#9660=AXIS2_PLACEMENT_3D('',#14768,#11729,#11730);
#9661=AXIS2_PLACEMENT_3D('',#14770,#11731,#11732);
#9662=AXIS2_PLACEMENT_3D('',#14773,#11734,#11735);
#9663=AXIS2_PLACEMENT_3D('',#14774,#11736,#11737);
#9664=AXIS2_PLACEMENT_3D('',#14776,#11738,#11739);
#9665=AXIS2_PLACEMENT_3D('',#14779,#11741,#11742);
#9666=AXIS2_PLACEMENT_3D('',#14780,#11743,#11744);
#9667=AXIS2_PLACEMENT_3D('',#14781,#11745,#11746);
#9668=AXIS2_PLACEMENT_3D('',#14782,#11747,#11748);
#9669=AXIS2_PLACEMENT_3D('',#14783,#11749,#11750);
#9670=AXIS2_PLACEMENT_3D('',#14785,#11751,#11752);
#9671=AXIS2_PLACEMENT_3D('',#14788,#11754,#11755);
#9672=AXIS2_PLACEMENT_3D('',#14789,#11756,#11757);
#9673=AXIS2_PLACEMENT_3D('',#14791,#11758,#11759);
#9674=AXIS2_PLACEMENT_3D('',#14794,#11761,#11762);
#9675=AXIS2_PLACEMENT_3D('',#14795,#11763,#11764);
#9676=AXIS2_PLACEMENT_3D('',#14796,#11765,#11766);
#9677=AXIS2_PLACEMENT_3D('',#14797,#11767,#11768);
#9678=AXIS2_PLACEMENT_3D('',#14798,#11769,#11770);
#9679=AXIS2_PLACEMENT_3D('',#14800,#11771,#11772);
#9680=AXIS2_PLACEMENT_3D('',#14803,#11774,#11775);
#9681=AXIS2_PLACEMENT_3D('',#14804,#11776,#11777);
#9682=AXIS2_PLACEMENT_3D('',#14806,#11778,#11779);
#9683=AXIS2_PLACEMENT_3D('',#14809,#11781,#11782);
#9684=AXIS2_PLACEMENT_3D('',#14810,#11783,#11784);
#9685=AXIS2_PLACEMENT_3D('',#14811,#11785,#11786);
#9686=AXIS2_PLACEMENT_3D('',#14812,#11787,#11788);
#9687=AXIS2_PLACEMENT_3D('',#14813,#11789,#11790);
#9688=AXIS2_PLACEMENT_3D('',#14814,#11791,#11792);
#9689=AXIS2_PLACEMENT_3D('',#14816,#11793,#11794);
#9690=AXIS2_PLACEMENT_3D('',#14819,#11796,#11797);
#9691=AXIS2_PLACEMENT_3D('',#14820,#11798,#11799);
#9692=AXIS2_PLACEMENT_3D('',#14822,#11800,#11801);
#9693=AXIS2_PLACEMENT_3D('',#14825,#11803,#11804);
#9694=AXIS2_PLACEMENT_3D('',#14826,#11805,#11806);
#9695=AXIS2_PLACEMENT_3D('',#14828,#11807,#11808);
#9696=AXIS2_PLACEMENT_3D('',#14831,#11810,#11811);
#9697=AXIS2_PLACEMENT_3D('',#14832,#11812,#11813);
#9698=AXIS2_PLACEMENT_3D('',#14834,#11814,#11815);
#9699=AXIS2_PLACEMENT_3D('',#14837,#11817,#11818);
#9700=AXIS2_PLACEMENT_3D('',#14838,#11819,#11820);
#9701=AXIS2_PLACEMENT_3D('',#14840,#11821,#11822);
#9702=AXIS2_PLACEMENT_3D('',#14843,#11824,#11825);
#9703=AXIS2_PLACEMENT_3D('',#14844,#11826,#11827);
#9704=AXIS2_PLACEMENT_3D('',#14846,#11828,#11829);
#9705=AXIS2_PLACEMENT_3D('',#14849,#11831,#11832);
#9706=AXIS2_PLACEMENT_3D('',#14850,#11833,#11834);
#9707=AXIS2_PLACEMENT_3D('',#14859,#11839,#11840);
#9708=AXIS2_PLACEMENT_3D('',#14868,#11845,#11846);
#9709=AXIS2_PLACEMENT_3D('',#14871,#11849,#11850);
#9710=AXIS2_PLACEMENT_3D('',#14873,#11852,#11853);
#9711=AXIS2_PLACEMENT_3D('',#14875,#11855,#11856);
#9712=AXIS2_PLACEMENT_3D('',#14884,#11861,#11862);
#9713=AXIS2_PLACEMENT_3D('',#14893,#11867,#11868);
#9714=AXIS2_PLACEMENT_3D('',#14896,#11871,#11872);
#9715=AXIS2_PLACEMENT_3D('',#14898,#11874,#11875);
#9716=AXIS2_PLACEMENT_3D('',#14900,#11877,#11878);
#9717=AXIS2_PLACEMENT_3D('',#14909,#11883,#11884);
#9718=AXIS2_PLACEMENT_3D('',#14915,#11888,#11889);
#9719=AXIS2_PLACEMENT_3D('',#14921,#11893,#11894);
#9720=AXIS2_PLACEMENT_3D('',#14924,#11897,#11898);
#9721=AXIS2_PLACEMENT_3D('',#14925,#11899,#11900);
#9722=AXIS2_PLACEMENT_3D('',#14926,#11901,#11902);
#9723=AXIS2_PLACEMENT_3D('',#14927,#11903,#11904);
#9724=AXIS2_PLACEMENT_3D('',#14929,#11905,#11906);
#9725=AXIS2_PLACEMENT_3D('',#14932,#11908,#11909);
#9726=AXIS2_PLACEMENT_3D('',#14933,#11910,#11911);
#9727=AXIS2_PLACEMENT_3D('',#14934,#11912,#11913);
#9728=AXIS2_PLACEMENT_3D('',#14936,#11914,#11915);
#9729=AXIS2_PLACEMENT_3D('',#14938,#11916,#11917);
#9730=AXIS2_PLACEMENT_3D('',#14939,#11918,#11919);
#9731=AXIS2_PLACEMENT_3D('',#14942,#11921,#11922);
#9732=AXIS2_PLACEMENT_3D('',#14943,#11923,#11924);
#9733=AXIS2_PLACEMENT_3D('',#14944,#11925,#11926);
#9734=AXIS2_PLACEMENT_3D('',#14946,#11927,#11928);
#9735=AXIS2_PLACEMENT_3D('',#14948,#11930,#11931);
#9736=AXIS2_PLACEMENT_3D('',#14949,#11932,#11933);
#9737=AXIS2_PLACEMENT_3D('',#14950,#11934,#11935);
#9738=AXIS2_PLACEMENT_3D('',#14952,#11936,#11937);
#9739=AXIS2_PLACEMENT_3D('',#14955,#11939,#11940);
#9740=AXIS2_PLACEMENT_3D('',#14956,#11941,#11942);
#9741=AXIS2_PLACEMENT_3D('',#14958,#11943,#11944);
#9742=AXIS2_PLACEMENT_3D('',#14961,#11946,#11947);
#9743=AXIS2_PLACEMENT_3D('',#14962,#11948,#11949);
#9744=AXIS2_PLACEMENT_3D('',#14963,#11950,#11951);
#9745=AXIS2_PLACEMENT_3D('',#14964,#11952,#11953);
#9746=AXIS2_PLACEMENT_3D('',#14965,#11954,#11955);
#9747=AXIS2_PLACEMENT_3D('',#14967,#11956,#11957);
#9748=AXIS2_PLACEMENT_3D('',#14970,#11959,#11960);
#9749=AXIS2_PLACEMENT_3D('',#14971,#11961,#11962);
#9750=AXIS2_PLACEMENT_3D('',#14973,#11963,#11964);
#9751=AXIS2_PLACEMENT_3D('',#14976,#11966,#11967);
#9752=AXIS2_PLACEMENT_3D('',#14977,#11968,#11969);
#9753=AXIS2_PLACEMENT_3D('',#14978,#11970,#11971);
#9754=AXIS2_PLACEMENT_3D('',#14979,#11972,#11973);
#9755=AXIS2_PLACEMENT_3D('',#14980,#11974,#11975);
#9756=AXIS2_PLACEMENT_3D('',#14982,#11976,#11977);
#9757=AXIS2_PLACEMENT_3D('',#14985,#11979,#11980);
#9758=AXIS2_PLACEMENT_3D('',#14986,#11981,#11982);
#9759=AXIS2_PLACEMENT_3D('',#14988,#11983,#11984);
#9760=AXIS2_PLACEMENT_3D('',#14991,#11986,#11987);
#9761=AXIS2_PLACEMENT_3D('',#14992,#11988,#11989);
#9762=AXIS2_PLACEMENT_3D('',#14993,#11990,#11991);
#9763=AXIS2_PLACEMENT_3D('',#14994,#11992,#11993);
#9764=AXIS2_PLACEMENT_3D('',#14995,#11994,#11995);
#9765=AXIS2_PLACEMENT_3D('',#14996,#11996,#11997);
#9766=AXIS2_PLACEMENT_3D('',#14998,#11998,#11999);
#9767=AXIS2_PLACEMENT_3D('',#15001,#12001,#12002);
#9768=AXIS2_PLACEMENT_3D('',#15002,#12003,#12004);
#9769=AXIS2_PLACEMENT_3D('',#15004,#12005,#12006);
#9770=AXIS2_PLACEMENT_3D('',#15007,#12008,#12009);
#9771=AXIS2_PLACEMENT_3D('',#15008,#12010,#12011);
#9772=AXIS2_PLACEMENT_3D('',#15010,#12012,#12013);
#9773=AXIS2_PLACEMENT_3D('',#15013,#12015,#12016);
#9774=AXIS2_PLACEMENT_3D('',#15014,#12017,#12018);
#9775=AXIS2_PLACEMENT_3D('',#15016,#12019,#12020);
#9776=AXIS2_PLACEMENT_3D('',#15019,#12022,#12023);
#9777=AXIS2_PLACEMENT_3D('',#15020,#12024,#12025);
#9778=AXIS2_PLACEMENT_3D('',#15022,#12026,#12027);
#9779=AXIS2_PLACEMENT_3D('',#15025,#12029,#12030);
#9780=AXIS2_PLACEMENT_3D('',#15026,#12031,#12032);
#9781=AXIS2_PLACEMENT_3D('',#15028,#12033,#12034);
#9782=AXIS2_PLACEMENT_3D('',#15031,#12036,#12037);
#9783=AXIS2_PLACEMENT_3D('',#15032,#12038,#12039);
#9784=AXIS2_PLACEMENT_3D('',#15041,#12044,#12045);
#9785=AXIS2_PLACEMENT_3D('',#15050,#12050,#12051);
#9786=AXIS2_PLACEMENT_3D('',#15053,#12054,#12055);
#9787=AXIS2_PLACEMENT_3D('',#15055,#12057,#12058);
#9788=AXIS2_PLACEMENT_3D('',#15057,#12060,#12061);
#9789=AXIS2_PLACEMENT_3D('',#15066,#12066,#12067);
#9790=AXIS2_PLACEMENT_3D('',#15075,#12072,#12073);
#9791=AXIS2_PLACEMENT_3D('',#15078,#12076,#12077);
#9792=AXIS2_PLACEMENT_3D('',#15080,#12079,#12080);
#9793=AXIS2_PLACEMENT_3D('',#15082,#12082,#12083);
#9794=AXIS2_PLACEMENT_3D('',#15091,#12088,#12089);
#9795=AXIS2_PLACEMENT_3D('',#15097,#12093,#12094);
#9796=AXIS2_PLACEMENT_3D('',#15103,#12098,#12099);
#9797=AXIS2_PLACEMENT_3D('',#15106,#12102,#12103);
#9798=AXIS2_PLACEMENT_3D('',#15107,#12104,#12105);
#9799=AXIS2_PLACEMENT_3D('',#15108,#12106,#12107);
#9800=AXIS2_PLACEMENT_3D('',#15109,#12108,#12109);
#9801=AXIS2_PLACEMENT_3D('',#15111,#12110,#12111);
#9802=AXIS2_PLACEMENT_3D('',#15114,#12113,#12114);
#9803=AXIS2_PLACEMENT_3D('',#15115,#12115,#12116);
#9804=AXIS2_PLACEMENT_3D('',#15116,#12117,#12118);
#9805=AXIS2_PLACEMENT_3D('',#15118,#12119,#12120);
#9806=AXIS2_PLACEMENT_3D('',#15120,#12121,#12122);
#9807=AXIS2_PLACEMENT_3D('',#15121,#12123,#12124);
#9808=AXIS2_PLACEMENT_3D('',#15124,#12126,#12127);
#9809=AXIS2_PLACEMENT_3D('',#15125,#12128,#12129);
#9810=AXIS2_PLACEMENT_3D('',#15126,#12130,#12131);
#9811=AXIS2_PLACEMENT_3D('',#15128,#12132,#12133);
#9812=AXIS2_PLACEMENT_3D('',#15130,#12135,#12136);
#9813=AXIS2_PLACEMENT_3D('',#15131,#12137,#12138);
#9814=AXIS2_PLACEMENT_3D('',#15132,#12139,#12140);
#9815=AXIS2_PLACEMENT_3D('',#15134,#12141,#12142);
#9816=AXIS2_PLACEMENT_3D('',#15137,#12144,#12145);
#9817=AXIS2_PLACEMENT_3D('',#15138,#12146,#12147);
#9818=AXIS2_PLACEMENT_3D('',#15140,#12148,#12149);
#9819=AXIS2_PLACEMENT_3D('',#15143,#12151,#12152);
#9820=AXIS2_PLACEMENT_3D('',#15144,#12153,#12154);
#9821=AXIS2_PLACEMENT_3D('',#15145,#12155,#12156);
#9822=AXIS2_PLACEMENT_3D('',#15146,#12157,#12158);
#9823=AXIS2_PLACEMENT_3D('',#15147,#12159,#12160);
#9824=AXIS2_PLACEMENT_3D('',#15149,#12161,#12162);
#9825=AXIS2_PLACEMENT_3D('',#15152,#12164,#12165);
#9826=AXIS2_PLACEMENT_3D('',#15153,#12166,#12167);
#9827=AXIS2_PLACEMENT_3D('',#15155,#12168,#12169);
#9828=AXIS2_PLACEMENT_3D('',#15158,#12171,#12172);
#9829=AXIS2_PLACEMENT_3D('',#15159,#12173,#12174);
#9830=AXIS2_PLACEMENT_3D('',#15160,#12175,#12176);
#9831=AXIS2_PLACEMENT_3D('',#15161,#12177,#12178);
#9832=AXIS2_PLACEMENT_3D('',#15162,#12179,#12180);
#9833=AXIS2_PLACEMENT_3D('',#15164,#12181,#12182);
#9834=AXIS2_PLACEMENT_3D('',#15167,#12184,#12185);
#9835=AXIS2_PLACEMENT_3D('',#15168,#12186,#12187);
#9836=AXIS2_PLACEMENT_3D('',#15170,#12188,#12189);
#9837=AXIS2_PLACEMENT_3D('',#15173,#12191,#12192);
#9838=AXIS2_PLACEMENT_3D('',#15174,#12193,#12194);
#9839=AXIS2_PLACEMENT_3D('',#15175,#12195,#12196);
#9840=AXIS2_PLACEMENT_3D('',#15176,#12197,#12198);
#9841=AXIS2_PLACEMENT_3D('',#15177,#12199,#12200);
#9842=AXIS2_PLACEMENT_3D('',#15186,#12205,#12206);
#9843=AXIS2_PLACEMENT_3D('',#15192,#12210,#12211);
#9844=AXIS2_PLACEMENT_3D('',#15198,#12215,#12216);
#9845=AXIS2_PLACEMENT_3D('',#15204,#12220,#12221);
#9846=AXIS2_PLACEMENT_3D('',#15210,#12225,#12226);
#9847=AXIS2_PLACEMENT_3D('',#15213,#12229,#12230);
#9848=AXIS2_PLACEMENT_3D('',#15214,#12231,#12232);
#9849=AXIS2_PLACEMENT_3D('',#15215,#12233,#12234);
#9850=AXIS2_PLACEMENT_3D('',#15217,#12235,#12236);
#9851=AXIS2_PLACEMENT_3D('',#15218,#12237,#12238);
#9852=AXIS2_PLACEMENT_3D('',#15220,#12239,#12240);
#9853=AXIS2_PLACEMENT_3D('',#15221,#12241,#12242);
#9854=AXIS2_PLACEMENT_3D('',#15223,#12243,#12244);
#9855=AXIS2_PLACEMENT_3D('',#15225,#12246,#12247);
#9856=AXIS2_PLACEMENT_3D('',#15227,#12248,#12249);
#9857=AXIS2_PLACEMENT_3D('',#15229,#12251,#12252);
#9858=AXIS2_PLACEMENT_3D('',#15231,#12253,#12254);
#9859=AXIS2_PLACEMENT_3D('',#15233,#12256,#12257);
#9860=AXIS2_PLACEMENT_3D('',#15235,#12258,#12259);
#9861=AXIS2_PLACEMENT_3D('',#15236,#12260,#12261);
#9862=AXIS2_PLACEMENT_3D('',#15238,#12262,#12263);
#9863=AXIS2_PLACEMENT_3D('',#15240,#12265,#12266);
#9864=AXIS2_PLACEMENT_3D('',#15242,#12268,#12269);
#9865=AXIS2_PLACEMENT_3D('',#15243,#12270,#12271);
#9866=AXIS2_PLACEMENT_3D('',#15252,#12276,#12277);
#9867=AXIS2_PLACEMENT_3D('',#15258,#12281,#12282);
#9868=AXIS2_PLACEMENT_3D('',#15264,#12286,#12287);
#9869=AXIS2_PLACEMENT_3D('',#15270,#12291,#12292);
#9870=AXIS2_PLACEMENT_3D('',#15276,#12296,#12297);
#9871=AXIS2_PLACEMENT_3D('',#15279,#12300,#12301);
#9872=AXIS2_PLACEMENT_3D('',#15280,#12302,#12303);
#9873=AXIS2_PLACEMENT_3D('',#15281,#12304,#12305);
#9874=AXIS2_PLACEMENT_3D('',#15283,#12306,#12307);
#9875=AXIS2_PLACEMENT_3D('',#15284,#12308,#12309);
#9876=AXIS2_PLACEMENT_3D('',#15286,#12310,#12311);
#9877=AXIS2_PLACEMENT_3D('',#15287,#12312,#12313);
#9878=AXIS2_PLACEMENT_3D('',#15289,#12314,#12315);
#9879=AXIS2_PLACEMENT_3D('',#15291,#12317,#12318);
#9880=AXIS2_PLACEMENT_3D('',#15293,#12319,#12320);
#9881=AXIS2_PLACEMENT_3D('',#15295,#12322,#12323);
#9882=AXIS2_PLACEMENT_3D('',#15297,#12324,#12325);
#9883=AXIS2_PLACEMENT_3D('',#15299,#12327,#12328);
#9884=AXIS2_PLACEMENT_3D('',#15301,#12329,#12330);
#9885=AXIS2_PLACEMENT_3D('',#15302,#12331,#12332);
#9886=AXIS2_PLACEMENT_3D('',#15304,#12333,#12334);
#9887=AXIS2_PLACEMENT_3D('',#15306,#12336,#12337);
#9888=AXIS2_PLACEMENT_3D('',#15308,#12339,#12340);
#9889=AXIS2_PLACEMENT_3D('',#15309,#12341,#12342);
#9890=AXIS2_PLACEMENT_3D('',#15310,#12343,#12344);
#9891=AXIS2_PLACEMENT_3D('',#15311,#12345,#12346);
#9892=AXIS2_PLACEMENT_3D('',#15312,#12347,#12348);
#9893=AXIS2_PLACEMENT_3D('',#15313,#12349,#12350);
#9894=AXIS2_PLACEMENT_3D('',#15314,#12351,#12352);
#9895=AXIS2_PLACEMENT_3D('',#15315,#12353,#12354);
#9896=AXIS2_PLACEMENT_3D('',#15316,#12355,#12356);
#9897=AXIS2_PLACEMENT_3D('',#15317,#12357,#12358);
#9898=AXIS2_PLACEMENT_3D('',#15318,#12359,#12360);
#9899=AXIS2_PLACEMENT_3D('',#15319,#12361,#12362);
#9900=AXIS2_PLACEMENT_3D('',#15320,#12363,#12364);
#9901=AXIS2_PLACEMENT_3D('',#15321,#12365,#12366);
#9902=AXIS2_PLACEMENT_3D('',#15322,#12367,#12368);
#9903=AXIS2_PLACEMENT_3D('',#15323,#12369,#12370);
#9904=AXIS2_PLACEMENT_3D('',#15324,#12371,#12372);
#9905=AXIS2_PLACEMENT_3D('',#15325,#12373,#12374);
#9906=AXIS2_PLACEMENT_3D('',#15326,#12375,#12376);
#9907=AXIS2_PLACEMENT_3D('',#15327,#12377,#12378);
#9908=AXIS2_PLACEMENT_3D('',#15328,#12379,#12380);
#9909=AXIS2_PLACEMENT_3D('',#15329,#12381,#12382);
#9910=AXIS2_PLACEMENT_3D('',#15330,#12383,#12384);
#9911=AXIS2_PLACEMENT_3D('',#15331,#12385,#12386);
#9912=AXIS2_PLACEMENT_3D('',#15332,#12387,#12388);
#9913=AXIS2_PLACEMENT_3D('',#15333,#12389,#12390);
#9914=AXIS2_PLACEMENT_3D('',#15334,#12391,#12392);
#9915=AXIS2_PLACEMENT_3D('',#15335,#12393,#12394);
#9916=AXIS2_PLACEMENT_3D('',#15336,#12395,#12396);
#9917=AXIS2_PLACEMENT_3D('',#15337,#12397,#12398);
#9918=AXIS2_PLACEMENT_3D('',#15338,#12399,#12400);
#9919=AXIS2_PLACEMENT_3D('',#15339,#12401,#12402);
#9920=AXIS2_PLACEMENT_3D('',#15340,#12403,#12404);
#9921=AXIS2_PLACEMENT_3D('',#15341,#12405,#12406);
#9922=AXIS2_PLACEMENT_3D('',#15342,#12407,#12408);
#9923=AXIS2_PLACEMENT_3D('',#15343,#12409,#12410);
#9924=AXIS2_PLACEMENT_3D('',#15344,#12411,#12412);
#9925=AXIS2_PLACEMENT_3D('',#15345,#12413,#12414);
#9926=AXIS2_PLACEMENT_3D('',#15346,#12415,#12416);
#9927=AXIS2_PLACEMENT_3D('',#15347,#12417,#12418);
#9928=AXIS2_PLACEMENT_3D('',#15348,#12419,#12420);
#9929=AXIS2_PLACEMENT_3D('',#15349,#12421,#12422);
#9930=AXIS2_PLACEMENT_3D('',#15350,#12423,#12424);
#9931=AXIS2_PLACEMENT_3D('',#15352,#12425,#12426);
#9932=AXIS2_PLACEMENT_3D('',#15355,#12428,#12429);
#9933=AXIS2_PLACEMENT_3D('',#15356,#12430,#12431);
#9934=AXIS2_PLACEMENT_3D('',#15358,#12432,#12433);
#9935=AXIS2_PLACEMENT_3D('',#15361,#12435,#12436);
#9936=AXIS2_PLACEMENT_3D('',#15362,#12437,#12438);
#9937=AXIS2_PLACEMENT_3D('',#15363,#12439,#12440);
#9938=AXIS2_PLACEMENT_3D('',#15364,#12441,#12442);
#9939=AXIS2_PLACEMENT_3D('',#15365,#12443,#12444);
#9940=AXIS2_PLACEMENT_3D('',#15367,#12445,#12446);
#9941=AXIS2_PLACEMENT_3D('',#15370,#12448,#12449);
#9942=AXIS2_PLACEMENT_3D('',#15371,#12450,#12451);
#9943=AXIS2_PLACEMENT_3D('',#15373,#12452,#12453);
#9944=AXIS2_PLACEMENT_3D('',#15376,#12455,#12456);
#9945=AXIS2_PLACEMENT_3D('',#15377,#12457,#12458);
#9946=AXIS2_PLACEMENT_3D('',#15378,#12459,#12460);
#9947=AXIS2_PLACEMENT_3D('',#15379,#12461,#12462);
#9948=AXIS2_PLACEMENT_3D('',#15380,#12463,#12464);
#9949=AXIS2_PLACEMENT_3D('',#15382,#12465,#12466);
#9950=AXIS2_PLACEMENT_3D('',#15385,#12468,#12469);
#9951=AXIS2_PLACEMENT_3D('',#15386,#12470,#12471);
#9952=AXIS2_PLACEMENT_3D('',#15388,#12472,#12473);
#9953=AXIS2_PLACEMENT_3D('',#15391,#12475,#12476);
#9954=AXIS2_PLACEMENT_3D('',#15392,#12477,#12478);
#9955=AXIS2_PLACEMENT_3D('',#15393,#12479,#12480);
#9956=AXIS2_PLACEMENT_3D('',#15394,#12481,#12482);
#9957=AXIS2_PLACEMENT_3D('',#15395,#12483,#12484);
#9958=AXIS2_PLACEMENT_3D('',#15396,#12485,#12486);
#9959=AXIS2_PLACEMENT_3D('',#15398,#12487,#12488);
#9960=AXIS2_PLACEMENT_3D('',#15401,#12490,#12491);
#9961=AXIS2_PLACEMENT_3D('',#15402,#12492,#12493);
#9962=AXIS2_PLACEMENT_3D('',#15404,#12494,#12495);
#9963=AXIS2_PLACEMENT_3D('',#15407,#12497,#12498);
#9964=AXIS2_PLACEMENT_3D('',#15408,#12499,#12500);
#9965=AXIS2_PLACEMENT_3D('',#15409,#12501,#12502);
#9966=AXIS2_PLACEMENT_3D('',#15410,#12503,#12504);
#9967=AXIS2_PLACEMENT_3D('',#15411,#12505,#12506);
#9968=AXIS2_PLACEMENT_3D('',#15413,#12507,#12508);
#9969=AXIS2_PLACEMENT_3D('',#15416,#12510,#12511);
#9970=AXIS2_PLACEMENT_3D('',#15417,#12512,#12513);
#9971=AXIS2_PLACEMENT_3D('',#15419,#12514,#12515);
#9972=AXIS2_PLACEMENT_3D('',#15422,#12517,#12518);
#9973=AXIS2_PLACEMENT_3D('',#15423,#12519,#12520);
#9974=AXIS2_PLACEMENT_3D('',#15424,#12521,#12522);
#9975=AXIS2_PLACEMENT_3D('',#15425,#12523,#12524);
#9976=AXIS2_PLACEMENT_3D('',#15426,#12525,#12526);
#9977=AXIS2_PLACEMENT_3D('',#15428,#12527,#12528);
#9978=AXIS2_PLACEMENT_3D('',#15431,#12530,#12531);
#9979=AXIS2_PLACEMENT_3D('',#15432,#12532,#12533);
#9980=AXIS2_PLACEMENT_3D('',#15434,#12534,#12535);
#9981=AXIS2_PLACEMENT_3D('',#15437,#12537,#12538);
#9982=AXIS2_PLACEMENT_3D('',#15438,#12539,#12540);
#9983=AXIS2_PLACEMENT_3D('',#15439,#12541,#12542);
#9984=AXIS2_PLACEMENT_3D('',#15440,#12543,#12544);
#9985=AXIS2_PLACEMENT_3D('',#15441,#12545,#12546);
#9986=AXIS2_PLACEMENT_3D('',#15442,#12547,#12548);
#9987=AXIS2_PLACEMENT_3D('',#15444,#12549,#12550);
#9988=AXIS2_PLACEMENT_3D('',#15447,#12552,#12553);
#9989=AXIS2_PLACEMENT_3D('',#15448,#12554,#12555);
#9990=AXIS2_PLACEMENT_3D('',#15450,#12556,#12557);
#9991=AXIS2_PLACEMENT_3D('',#15453,#12559,#12560);
#9992=AXIS2_PLACEMENT_3D('',#15454,#12561,#12562);
#9993=AXIS2_PLACEMENT_3D('',#15455,#12563,#12564);
#9994=AXIS2_PLACEMENT_3D('',#15456,#12565,#12566);
#9995=AXIS2_PLACEMENT_3D('',#15457,#12567,#12568);
#9996=AXIS2_PLACEMENT_3D('',#15459,#12569,#12570);
#9997=AXIS2_PLACEMENT_3D('',#15462,#12572,#12573);
#9998=AXIS2_PLACEMENT_3D('',#15463,#12574,#12575);
#9999=AXIS2_PLACEMENT_3D('',#15465,#12576,#12577);
#10000=AXIS2_PLACEMENT_3D('',#15468,#12579,#12580);
#10001=AXIS2_PLACEMENT_3D('',#15469,#12581,#12582);
#10002=AXIS2_PLACEMENT_3D('',#15470,#12583,#12584);
#10003=AXIS2_PLACEMENT_3D('',#15471,#12585,#12586);
#10004=AXIS2_PLACEMENT_3D('',#15472,#12587,#12588);
#10005=AXIS2_PLACEMENT_3D('',#15474,#12589,#12590);
#10006=AXIS2_PLACEMENT_3D('',#15477,#12592,#12593);
#10007=AXIS2_PLACEMENT_3D('',#15478,#12594,#12595);
#10008=AXIS2_PLACEMENT_3D('',#15480,#12596,#12597);
#10009=AXIS2_PLACEMENT_3D('',#15483,#12599,#12600);
#10010=AXIS2_PLACEMENT_3D('',#15484,#12601,#12602);
#10011=AXIS2_PLACEMENT_3D('',#15485,#12603,#12604);
#10012=AXIS2_PLACEMENT_3D('',#15486,#12605,#12606);
#10013=AXIS2_PLACEMENT_3D('',#15487,#12607,#12608);
#10014=AXIS2_PLACEMENT_3D('',#15488,#12609,#12610);
#10015=AXIS2_PLACEMENT_3D('',#15490,#12611,#12612);
#10016=AXIS2_PLACEMENT_3D('',#15493,#12614,#12615);
#10017=AXIS2_PLACEMENT_3D('',#15494,#12616,#12617);
#10018=AXIS2_PLACEMENT_3D('',#15496,#12618,#12619);
#10019=AXIS2_PLACEMENT_3D('',#15499,#12621,#12622);
#10020=AXIS2_PLACEMENT_3D('',#15500,#12623,#12624);
#10021=AXIS2_PLACEMENT_3D('',#15501,#12625,#12626);
#10022=AXIS2_PLACEMENT_3D('',#15502,#12627,#12628);
#10023=AXIS2_PLACEMENT_3D('',#15503,#12629,#12630);
#10024=AXIS2_PLACEMENT_3D('',#15505,#12631,#12632);
#10025=AXIS2_PLACEMENT_3D('',#15508,#12634,#12635);
#10026=AXIS2_PLACEMENT_3D('',#15509,#12636,#12637);
#10027=AXIS2_PLACEMENT_3D('',#15511,#12638,#12639);
#10028=AXIS2_PLACEMENT_3D('',#15514,#12641,#12642);
#10029=AXIS2_PLACEMENT_3D('',#15515,#12643,#12644);
#10030=AXIS2_PLACEMENT_3D('',#15516,#12645,#12646);
#10031=AXIS2_PLACEMENT_3D('',#15517,#12647,#12648);
#10032=AXIS2_PLACEMENT_3D('',#15518,#12649,#12650);
#10033=AXIS2_PLACEMENT_3D('',#15520,#12651,#12652);
#10034=AXIS2_PLACEMENT_3D('',#15523,#12654,#12655);
#10035=AXIS2_PLACEMENT_3D('',#15524,#12656,#12657);
#10036=AXIS2_PLACEMENT_3D('',#15526,#12658,#12659);
#10037=AXIS2_PLACEMENT_3D('',#15529,#12661,#12662);
#10038=AXIS2_PLACEMENT_3D('',#15530,#12663,#12664);
#10039=AXIS2_PLACEMENT_3D('',#15531,#12665,#12666);
#10040=AXIS2_PLACEMENT_3D('',#15532,#12667,#12668);
#10041=AXIS2_PLACEMENT_3D('',#15533,#12669,#12670);
#10042=AXIS2_PLACEMENT_3D('',#15534,#12671,#12672);
#10043=AXIS2_PLACEMENT_3D('',#15537,#12673,#12674);
#10044=AXIS2_PLACEMENT_3D('',#15538,#12675,#12676);
#10045=AXIS2_PLACEMENT_3D('',#15540,#12677,#12678);
#10046=AXIS2_PLACEMENT_3D('',#15542,#12679,#12680);
#10047=AXIS2_PLACEMENT_3D('',#15543,#12681,#12682);
#10048=AXIS2_PLACEMENT_3D('',#15544,#12683,#12684);
#10049=AXIS2_PLACEMENT_3D('',#15547,#12686,#12687);
#10050=AXIS2_PLACEMENT_3D('',#15548,#12688,#12689);
#10051=AXIS2_PLACEMENT_3D('',#15550,#12690,#12691);
#10052=AXIS2_PLACEMENT_3D('',#15553,#12693,#12694);
#10053=AXIS2_PLACEMENT_3D('',#15554,#12695,#12696);
#10054=AXIS2_PLACEMENT_3D('',#15557,#12698,#12699);
#10055=AXIS2_PLACEMENT_3D('',#15558,#12700,#12701);
#10056=AXIS2_PLACEMENT_3D('',#15559,#12702,#12703);
#10057=AXIS2_PLACEMENT_3D('',#15561,#12704,#12705);
#10058=AXIS2_PLACEMENT_3D('',#15563,#12707,#12708);
#10059=AXIS2_PLACEMENT_3D('',#15565,#12709,#12710);
#10060=AXIS2_PLACEMENT_3D('',#15566,#12711,#12712);
#10061=AXIS2_PLACEMENT_3D('',#15568,#12714,#12715);
#10062=AXIS2_PLACEMENT_3D('',#15569,#12716,#12717);
#10063=AXIS2_PLACEMENT_3D('',#15572,#12718,#12719);
#10064=AXIS2_PLACEMENT_3D('',#15573,#12720,#12721);
#10065=AXIS2_PLACEMENT_3D('',#15575,#12722,#12723);
#10066=AXIS2_PLACEMENT_3D('',#15577,#12724,#12725);
#10067=AXIS2_PLACEMENT_3D('',#15578,#12726,#12727);
#10068=AXIS2_PLACEMENT_3D('',#15579,#12728,#12729);
#10069=AXIS2_PLACEMENT_3D('',#15581,#12730,#12731);
#10070=AXIS2_PLACEMENT_3D('',#15583,#12733,#12734);
#10071=AXIS2_PLACEMENT_3D('',#15585,#12735,#12736);
#10072=AXIS2_PLACEMENT_3D('',#15587,#12737,#12738);
#10073=AXIS2_PLACEMENT_3D('',#15588,#12739,#12740);
#10074=AXIS2_PLACEMENT_3D('',#15590,#12741,#12742);
#10075=AXIS2_PLACEMENT_3D('',#15592,#12744,#12745);
#10076=AXIS2_PLACEMENT_3D('',#15594,#12746,#12747);
#10077=AXIS2_PLACEMENT_3D('',#15596,#12749,#12750);
#10078=AXIS2_PLACEMENT_3D('',#15598,#12751,#12752);
#10079=AXIS2_PLACEMENT_3D('',#15600,#12754,#12755);
#10080=AXIS2_PLACEMENT_3D('',#15601,#12756,#12757);
#10081=AXIS2_PLACEMENT_3D('',#15603,#12759,#12760);
#10082=AXIS2_PLACEMENT_3D('',#15604,#12761,#12762);
#10083=AXIS2_PLACEMENT_3D('',#15607,#12763,#12764);
#10084=AXIS2_PLACEMENT_3D('',#15608,#12765,#12766);
#10085=AXIS2_PLACEMENT_3D('',#15611,#12767,#12768);
#10086=AXIS2_PLACEMENT_3D('',#15612,#12769,#12770);
#10087=AXIS2_PLACEMENT_3D('',#15615,#12771,#12772);
#10088=AXIS2_PLACEMENT_3D('',#15616,#12773,#12774);
#10089=AXIS2_PLACEMENT_3D('',#15619,#12775,#12776);
#10090=AXIS2_PLACEMENT_3D('',#15620,#12777,#12778);
#10091=AXIS2_PLACEMENT_3D('',#15623,#12779,#12780);
#10092=AXIS2_PLACEMENT_3D('',#15624,#12781,#12782);
#10093=AXIS2_PLACEMENT_3D('',#15627,#12783,#12784);
#10094=AXIS2_PLACEMENT_3D('',#15628,#12785,#12786);
#10095=AXIS2_PLACEMENT_3D('',#15631,#12787,#12788);
#10096=AXIS2_PLACEMENT_3D('',#15632,#12789,#12790);
#10097=AXIS2_PLACEMENT_3D('',#15635,#12791,#12792);
#10098=AXIS2_PLACEMENT_3D('',#15636,#12793,#12794);
#10099=AXIS2_PLACEMENT_3D('',#15637,#12795,#12796);
#10100=AXIS2_PLACEMENT_3D('',#15663,#12797,#12798);
#10101=AXIS2_PLACEMENT_3D('',#15687,#12799,#12800);
#10102=AXIS2_PLACEMENT_3D('',#15688,#12801,#12802);
#10103=AXIS2_PLACEMENT_3D('',#15690,#12803,#12804);
#10104=AXIS2_PLACEMENT_3D('',#15715,#12805,#12806);
#10105=AXIS2_PLACEMENT_3D('',#15740,#12807,#12808);
#10106=AXIS2_PLACEMENT_3D('',#15756,#12810,#12811);
#10107=AXIS2_PLACEMENT_3D('',#15771,#12812,#12813);
#10108=AXIS2_PLACEMENT_3D('',#15796,#12814,#12815);
#10109=AXIS2_PLACEMENT_3D('',#15821,#12816,#12817);
#10110=AXIS2_PLACEMENT_3D('',#15846,#12818,#12819);
#10111=AXIS2_PLACEMENT_3D('',#15870,#12820,#12821);
#10112=AXIS2_PLACEMENT_3D('',#15871,#12822,#12823);
#10113=AXIS2_PLACEMENT_3D('',#15873,#12824,#12825);
#10114=AXIS2_PLACEMENT_3D('',#15874,#12826,#12827);
#10115=AXIS2_PLACEMENT_3D('',#15875,#12828,#12829);
#10116=AXIS2_PLACEMENT_3D('',#15899,#12830,#12831);
#10117=AXIS2_PLACEMENT_3D('',#15900,#12832,#12833);
#10118=AXIS2_PLACEMENT_3D('',#15902,#12834,#12835);
#10119=AXIS2_PLACEMENT_3D('',#15903,#12836,#12837);
#10120=AXIS2_PLACEMENT_3D('',#15904,#12838,#12839);
#10121=AXIS2_PLACEMENT_3D('',#15928,#12840,#12841);
#10122=AXIS2_PLACEMENT_3D('',#15929,#12842,#12843);
#10123=AXIS2_PLACEMENT_3D('',#15931,#12844,#12845);
#10124=AXIS2_PLACEMENT_3D('',#15932,#12846,#12847);
#10125=AXIS2_PLACEMENT_3D('',#15933,#12848,#12849);
#10126=AXIS2_PLACEMENT_3D('',#15948,#12850,#12851);
#10127=AXIS2_PLACEMENT_3D('',#15961,#12852,#12853);
#10128=AXIS2_PLACEMENT_3D('',#15963,#12854,#12855);
#10129=AXIS2_PLACEMENT_3D('',#15964,#12856,#12857);
#10130=AXIS2_PLACEMENT_3D('',#15965,#12858,#12859);
#10131=AXIS2_PLACEMENT_3D('',#15989,#12860,#12861);
#10132=AXIS2_PLACEMENT_3D('',#15990,#12862,#12863);
#10133=AXIS2_PLACEMENT_3D('',#15992,#12864,#12865);
#10134=AXIS2_PLACEMENT_3D('',#15993,#12866,#12867);
#10135=AXIS2_PLACEMENT_3D('',#15994,#12868,#12869);
#10136=AXIS2_PLACEMENT_3D('',#16018,#12870,#12871);
#10137=AXIS2_PLACEMENT_3D('',#16019,#12872,#12873);
#10138=AXIS2_PLACEMENT_3D('',#16021,#12874,#12875);
#10139=AXIS2_PLACEMENT_3D('',#16022,#12876,#12877);
#10140=AXIS2_PLACEMENT_3D('',#16023,#12878,#12879);
#10141=AXIS2_PLACEMENT_3D('',#16047,#12880,#12881);
#10142=AXIS2_PLACEMENT_3D('',#16048,#12882,#12883);
#10143=AXIS2_PLACEMENT_3D('',#16050,#12884,#12885);
#10144=AXIS2_PLACEMENT_3D('',#16053,#12887,#12888);
#10145=AXIS2_PLACEMENT_3D('',#16077,#12889,#12890);
#10146=AXIS2_PLACEMENT_3D('',#16078,#12891,#12892);
#10147=AXIS2_PLACEMENT_3D('',#16079,#12893,#12894);
#10148=AXIS2_PLACEMENT_3D('',#16080,#12895,#12896);
#10149=AXIS2_PLACEMENT_3D('',#16081,#12897,#12898);
#10150=AXIS2_PLACEMENT_3D('',#16082,#12899,#12900);
#10151=AXIS2_PLACEMENT_3D('',#16083,#12901,#12902);
#10152=AXIS2_PLACEMENT_3D('',#16084,#12903,#12904);
#10153=AXIS2_PLACEMENT_3D('',#16085,#12905,#12906);
#10154=AXIS2_PLACEMENT_3D('',#16087,#12907,#12908);
#10155=AXIS2_PLACEMENT_3D('',#16089,#12909,#12910);
#10156=AXIS2_PLACEMENT_3D('',#16090,#12911,#12912);
#10157=AXIS2_PLACEMENT_3D('',#16092,#12913,#12914);
#10158=AXIS2_PLACEMENT_3D('',#16094,#12916,#12917);
#10159=AXIS2_PLACEMENT_3D('',#16096,#12918,#12919);
#10160=AXIS2_PLACEMENT_3D('',#16097,#12920,#12921);
#10161=AXIS2_PLACEMENT_3D('',#16099,#12923,#12924);
#10162=AXIS2_PLACEMENT_3D('',#16101,#12925,#12926);
#10163=AXIS2_PLACEMENT_3D('',#16103,#12927,#12928);
#10164=AXIS2_PLACEMENT_3D('',#16104,#12929,#12930);
#10165=AXIS2_PLACEMENT_3D('',#16106,#12931,#12932);
#10166=AXIS2_PLACEMENT_3D('',#16108,#12934,#12935);
#10167=AXIS2_PLACEMENT_3D('',#16110,#12936,#12937);
#10168=AXIS2_PLACEMENT_3D('',#16111,#12938,#12939);
#10169=AXIS2_PLACEMENT_3D('',#16113,#12941,#12942);
#10170=AXIS2_PLACEMENT_3D('',#16114,#12943,#12944);
#10171=AXIS2_PLACEMENT_3D('',#16115,#12945,#12946);
#10172=AXIS2_PLACEMENT_3D('',#16116,#12947,#12948);
#10173=AXIS2_PLACEMENT_3D('',#16117,#12949,#12950);
#10174=AXIS2_PLACEMENT_3D('',#16118,#12951,#12952);
#10175=AXIS2_PLACEMENT_3D('',#16119,#12953,#12954);
#10176=AXIS2_PLACEMENT_3D('',#16120,#12955,#12956);
#10177=AXIS2_PLACEMENT_3D('',#16121,#12957,#12958);
#10178=AXIS2_PLACEMENT_3D('',#16122,#12959,#12960);
#10179=AXIS2_PLACEMENT_3D('',#16123,#12961,#12962);
#10180=AXIS2_PLACEMENT_3D('',#16124,#12963,#12964);
#10181=AXIS2_PLACEMENT_3D('',#16125,#12965,#12966);
#10182=AXIS2_PLACEMENT_3D('',#16126,#12967,#12968);
#10183=AXIS2_PLACEMENT_3D('',#16127,#12969,#12970);
#10184=AXIS2_PLACEMENT_3D('',#16128,#12971,#12972);
#10185=AXIS2_PLACEMENT_3D('',#16129,#12973,#12974);
#10186=AXIS2_PLACEMENT_3D('',#16130,#12975,#12976);
#10187=AXIS2_PLACEMENT_3D('',#16131,#12977,#12978);
#10188=AXIS2_PLACEMENT_3D('',#16132,#12979,#12980);
#10189=AXIS2_PLACEMENT_3D('',#16133,#12981,#12982);
#10190=AXIS2_PLACEMENT_3D('',#16134,#12983,#12984);
#10191=AXIS2_PLACEMENT_3D('',#16135,#12985,#12986);
#10192=AXIS2_PLACEMENT_3D('',#16136,#12987,#12988);
#10193=AXIS2_PLACEMENT_3D('',#16137,#12989,#12990);
#10194=AXIS2_PLACEMENT_3D('',#16138,#12991,#12992);
#10195=AXIS2_PLACEMENT_3D('',#16139,#12993,#12994);
#10196=AXIS2_PLACEMENT_3D('',#16140,#12995,#12996);
#10197=AXIS2_PLACEMENT_3D('',#16141,#12997,#12998);
#10198=AXIS2_PLACEMENT_3D('',#16142,#12999,#13000);
#10199=AXIS2_PLACEMENT_3D('',#16143,#13001,#13002);
#10200=DIRECTION('axis',(0.,0.,1.));
#10201=DIRECTION('refdir',(1.,0.,0.));
#10202=DIRECTION('axis',(0.,0.,1.));
#10203=DIRECTION('refdir',(1.,0.,0.));
#10204=DIRECTION('axis',(0.,0.,1.));
#10205=DIRECTION('refdir',(1.,0.,0.));
#10206=DIRECTION('center_axis',(0.,0.,1.));
#10207=DIRECTION('ref_axis',(1.,0.,0.));
#10208=DIRECTION('center_axis',(0.,0.,1.));
#10209=DIRECTION('ref_axis',(1.,0.,0.));
#10210=DIRECTION('',(0.,0.,1.));
#10211=DIRECTION('center_axis',(0.,0.,-1.));
#10212=DIRECTION('ref_axis',(1.,0.,0.));
#10213=DIRECTION('center_axis',(0.,0.,1.));
#10214=DIRECTION('ref_axis',(1.,0.,0.));
#10215=DIRECTION('center_axis',(0.,0.,1.));
#10216=DIRECTION('ref_axis',(1.,0.,0.));
#10217=DIRECTION('',(0.,0.,1.));
#10218=DIRECTION('center_axis',(0.,0.,-1.));
#10219=DIRECTION('ref_axis',(1.,0.,0.));
#10220=DIRECTION('center_axis',(0.,0.,1.));
#10221=DIRECTION('ref_axis',(1.,0.,0.));
#10222=DIRECTION('center_axis',(0.,0.,1.));
#10223=DIRECTION('ref_axis',(1.,0.,0.));
#10224=DIRECTION('',(0.,0.,1.));
#10225=DIRECTION('center_axis',(0.,0.,-1.));
#10226=DIRECTION('ref_axis',(1.,0.,0.));
#10227=DIRECTION('center_axis',(0.,0.,1.));
#10228=DIRECTION('ref_axis',(1.,0.,0.));
#10229=DIRECTION('center_axis',(0.,0.,1.));
#10230=DIRECTION('ref_axis',(1.,0.,0.));
#10231=DIRECTION('',(0.,0.,1.));
#10232=DIRECTION('center_axis',(0.,0.,-1.));
#10233=DIRECTION('ref_axis',(1.,0.,0.));
#10234=DIRECTION('center_axis',(0.,0.,1.));
#10235=DIRECTION('ref_axis',(1.,0.,0.));
#10236=DIRECTION('center_axis',(0.,0.,1.));
#10237=DIRECTION('ref_axis',(1.,0.,0.));
#10238=DIRECTION('',(0.,0.,1.));
#10239=DIRECTION('center_axis',(0.,0.,-1.));
#10240=DIRECTION('ref_axis',(1.,0.,0.));
#10241=DIRECTION('center_axis',(0.,0.,1.));
#10242=DIRECTION('ref_axis',(1.,0.,0.));
#10243=DIRECTION('center_axis',(0.,0.,1.));
#10244=DIRECTION('ref_axis',(1.,0.,0.));
#10245=DIRECTION('',(0.,0.,1.));
#10246=DIRECTION('center_axis',(0.,0.,-1.));
#10247=DIRECTION('ref_axis',(1.,0.,0.));
#10248=DIRECTION('center_axis',(0.,0.,1.));
#10249=DIRECTION('ref_axis',(1.,0.,0.));
#10250=DIRECTION('center_axis',(0.,0.,1.));
#10251=DIRECTION('ref_axis',(1.,0.,0.));
#10252=DIRECTION('',(0.,0.,1.));
#10253=DIRECTION('center_axis',(0.,0.,-1.));
#10254=DIRECTION('ref_axis',(1.,0.,0.));
#10255=DIRECTION('center_axis',(0.,0.,1.));
#10256=DIRECTION('ref_axis',(1.,0.,0.));
#10257=DIRECTION('center_axis',(0.,0.,1.));
#10258=DIRECTION('ref_axis',(1.,0.,0.));
#10259=DIRECTION('',(0.,0.,1.));
#10260=DIRECTION('center_axis',(0.,0.,-1.));
#10261=DIRECTION('ref_axis',(1.,0.,0.));
#10262=DIRECTION('center_axis',(0.,0.,1.));
#10263=DIRECTION('ref_axis',(1.,0.,0.));
#10264=DIRECTION('center_axis',(0.,0.,1.));
#10265=DIRECTION('ref_axis',(1.,0.,0.));
#10266=DIRECTION('',(0.,0.,1.));
#10267=DIRECTION('center_axis',(0.,0.,-1.));
#10268=DIRECTION('ref_axis',(1.,0.,0.));
#10269=DIRECTION('center_axis',(0.,0.,1.));
#10270=DIRECTION('ref_axis',(1.,0.,0.));
#10271=DIRECTION('center_axis',(0.,0.,1.));
#10272=DIRECTION('ref_axis',(1.,0.,0.));
#10273=DIRECTION('',(0.,0.,1.));
#10274=DIRECTION('center_axis',(0.,0.,-1.));
#10275=DIRECTION('ref_axis',(1.,0.,0.));
#10276=DIRECTION('center_axis',(0.,0.,1.));
#10277=DIRECTION('ref_axis',(1.,0.,0.));
#10278=DIRECTION('center_axis',(0.,0.,1.));
#10279=DIRECTION('ref_axis',(1.,0.,0.));
#10280=DIRECTION('',(0.,0.,1.));
#10281=DIRECTION('center_axis',(0.,0.,-1.));
#10282=DIRECTION('ref_axis',(1.,0.,0.));
#10283=DIRECTION('center_axis',(0.,0.,1.));
#10284=DIRECTION('ref_axis',(1.,0.,0.));
#10285=DIRECTION('center_axis',(0.,0.,1.));
#10286=DIRECTION('ref_axis',(1.,0.,0.));
#10287=DIRECTION('',(0.,0.,1.));
#10288=DIRECTION('center_axis',(0.,0.,-1.));
#10289=DIRECTION('ref_axis',(1.,0.,0.));
#10290=DIRECTION('center_axis',(0.,0.,1.));
#10291=DIRECTION('ref_axis',(1.,0.,0.));
#10292=DIRECTION('center_axis',(0.,0.,1.));
#10293=DIRECTION('ref_axis',(1.,0.,0.));
#10294=DIRECTION('',(0.,0.,1.));
#10295=DIRECTION('center_axis',(0.,0.,-1.));
#10296=DIRECTION('ref_axis',(1.,0.,0.));
#10297=DIRECTION('center_axis',(0.,0.,1.));
#10298=DIRECTION('ref_axis',(1.,0.,0.));
#10299=DIRECTION('center_axis',(0.,0.,1.));
#10300=DIRECTION('ref_axis',(1.,0.,0.));
#10301=DIRECTION('',(0.,0.,1.));
#10302=DIRECTION('center_axis',(0.,0.,-1.));
#10303=DIRECTION('ref_axis',(1.,0.,0.));
#10304=DIRECTION('center_axis',(0.,0.,1.));
#10305=DIRECTION('ref_axis',(1.,0.,0.));
#10306=DIRECTION('center_axis',(0.,0.,1.));
#10307=DIRECTION('ref_axis',(1.,0.,0.));
#10308=DIRECTION('',(0.,0.,1.));
#10309=DIRECTION('center_axis',(0.,0.,-1.));
#10310=DIRECTION('ref_axis',(1.,0.,0.));
#10311=DIRECTION('center_axis',(0.,0.,1.));
#10312=DIRECTION('ref_axis',(1.,0.,0.));
#10313=DIRECTION('center_axis',(0.,0.,1.));
#10314=DIRECTION('ref_axis',(1.,0.,0.));
#10315=DIRECTION('',(0.,0.,1.));
#10316=DIRECTION('center_axis',(0.,0.,-1.));
#10317=DIRECTION('ref_axis',(1.,0.,0.));
#10318=DIRECTION('center_axis',(0.,0.,1.));
#10319=DIRECTION('ref_axis',(1.,0.,0.));
#10320=DIRECTION('center_axis',(0.,0.,1.));
#10321=DIRECTION('ref_axis',(1.,0.,0.));
#10322=DIRECTION('',(0.,0.,1.));
#10323=DIRECTION('center_axis',(0.,0.,-1.));
#10324=DIRECTION('ref_axis',(1.,0.,0.));
#10325=DIRECTION('center_axis',(0.,0.,1.));
#10326=DIRECTION('ref_axis',(1.,0.,0.));
#10327=DIRECTION('center_axis',(0.,0.,1.));
#10328=DIRECTION('ref_axis',(1.,0.,0.));
#10329=DIRECTION('',(0.,0.,1.));
#10330=DIRECTION('center_axis',(0.,0.,-1.));
#10331=DIRECTION('ref_axis',(1.,0.,0.));
#10332=DIRECTION('center_axis',(0.,0.,1.));
#10333=DIRECTION('ref_axis',(1.,0.,0.));
#10334=DIRECTION('center_axis',(0.,0.,1.));
#10335=DIRECTION('ref_axis',(1.,0.,0.));
#10336=DIRECTION('',(0.,0.,1.));
#10337=DIRECTION('center_axis',(0.,0.,-1.));
#10338=DIRECTION('ref_axis',(1.,0.,0.));
#10339=DIRECTION('center_axis',(0.,0.,1.));
#10340=DIRECTION('ref_axis',(1.,0.,0.));
#10341=DIRECTION('center_axis',(0.,0.,1.));
#10342=DIRECTION('ref_axis',(1.,0.,0.));
#10343=DIRECTION('',(0.,0.,1.));
#10344=DIRECTION('center_axis',(0.,0.,-1.));
#10345=DIRECTION('ref_axis',(1.,0.,0.));
#10346=DIRECTION('center_axis',(0.,1.,0.));
#10347=DIRECTION('ref_axis',(-1.,0.,0.));
#10348=DIRECTION('',(-1.,0.,0.));
#10349=DIRECTION('',(0.,0.,1.));
#10350=DIRECTION('',(-1.,0.,0.));
#10351=DIRECTION('',(0.,0.,1.));
#10352=DIRECTION('center_axis',(1.,0.,0.));
#10353=DIRECTION('ref_axis',(0.,1.,0.));
#10354=DIRECTION('',(0.,1.,0.));
#10355=DIRECTION('',(0.,1.,0.));
#10356=DIRECTION('',(0.,0.,1.));
#10357=DIRECTION('center_axis',(0.,-1.,0.));
#10358=DIRECTION('ref_axis',(1.,0.,0.));
#10359=DIRECTION('',(1.,0.,0.));
#10360=DIRECTION('',(1.,0.,0.));
#10361=DIRECTION('',(0.,0.,1.));
#10362=DIRECTION('center_axis',(-1.,0.,0.));
#10363=DIRECTION('ref_axis',(0.,-1.,0.));
#10364=DIRECTION('',(0.,-1.,0.));
#10365=DIRECTION('',(0.,-1.,0.));
#10366=DIRECTION('center_axis',(0.,0.,1.));
#10367=DIRECTION('ref_axis',(1.,0.,0.));
#10368=DIRECTION('center_axis',(0.,0.,1.));
#10369=DIRECTION('ref_axis',(1.,0.,0.));
#10370=DIRECTION('axis',(0.,0.,1.));
#10371=DIRECTION('refdir',(1.,0.,0.));
#10372=DIRECTION('center_axis',(0.,0.,1.));
#10373=DIRECTION('ref_axis',(1.,0.,0.));
#10374=DIRECTION('',(0.,0.,1.));
#10375=DIRECTION('center_axis',(0.,0.,1.));
#10376=DIRECTION('ref_axis',(1.,0.,0.));
#10377=DIRECTION('',(0.,0.,1.));
#10378=DIRECTION('center_axis',(0.,0.,-1.));
#10379=DIRECTION('ref_axis',(1.,0.,0.));
#10380=DIRECTION('center_axis',(0.,0.,1.));
#10381=DIRECTION('ref_axis',(1.,0.,0.));
#10382=DIRECTION('',(0.,0.,1.));
#10383=DIRECTION('center_axis',(0.,0.,1.));
#10384=DIRECTION('ref_axis',(1.,0.,0.));
#10385=DIRECTION('',(0.,0.,1.));
#10386=DIRECTION('center_axis',(0.,0.,-1.));
#10387=DIRECTION('ref_axis',(1.,0.,0.));
#10388=DIRECTION('center_axis',(0.,0.,1.));
#10389=DIRECTION('ref_axis',(1.,0.,0.));
#10390=DIRECTION('',(0.,0.,1.));
#10391=DIRECTION('center_axis',(0.,0.,1.));
#10392=DIRECTION('ref_axis',(1.,0.,0.));
#10393=DIRECTION('',(0.,0.,1.));
#10394=DIRECTION('center_axis',(0.,0.,-1.));
#10395=DIRECTION('ref_axis',(1.,0.,0.));
#10396=DIRECTION('center_axis',(0.,0.,1.));
#10397=DIRECTION('ref_axis',(1.,0.,0.));
#10398=DIRECTION('',(0.,0.,1.));
#10399=DIRECTION('center_axis',(0.,0.,1.));
#10400=DIRECTION('ref_axis',(1.,0.,0.));
#10401=DIRECTION('',(0.,0.,1.));
#10402=DIRECTION('center_axis',(0.,0.,-1.));
#10403=DIRECTION('ref_axis',(1.,0.,0.));
#10404=DIRECTION('center_axis',(0.,0.,1.));
#10405=DIRECTION('ref_axis',(1.,0.,0.));
#10406=DIRECTION('center_axis',(0.,0.,1.));
#10407=DIRECTION('ref_axis',(1.,0.,0.));
#10408=DIRECTION('',(0.,0.,1.));
#10409=DIRECTION('center_axis',(0.,0.,-1.));
#10410=DIRECTION('ref_axis',(1.,0.,0.));
#10411=DIRECTION('center_axis',(0.,0.,1.));
#10412=DIRECTION('ref_axis',(1.,0.,0.));
#10413=DIRECTION('center_axis',(0.,0.,1.));
#10414=DIRECTION('ref_axis',(1.,0.,0.));
#10415=DIRECTION('center_axis',(0.,0.,1.));
#10416=DIRECTION('ref_axis',(1.,0.,0.));
#10417=DIRECTION('',(0.,0.,1.));
#10418=DIRECTION('center_axis',(0.,0.,-1.));
#10419=DIRECTION('ref_axis',(1.,0.,0.));
#10420=DIRECTION('center_axis',(0.,0.,1.));
#10421=DIRECTION('ref_axis',(1.,0.,0.));
#10422=DIRECTION('center_axis',(0.,0.,1.));
#10423=DIRECTION('ref_axis',(1.,0.,0.));
#10424=DIRECTION('center_axis',(0.,0.,1.));
#10425=DIRECTION('ref_axis',(1.,0.,0.));
#10426=DIRECTION('',(0.,0.,1.));
#10427=DIRECTION('center_axis',(0.,0.,-1.));
#10428=DIRECTION('ref_axis',(1.,0.,0.));
#10429=DIRECTION('center_axis',(0.,0.,1.));
#10430=DIRECTION('ref_axis',(1.,0.,0.));
#10431=DIRECTION('center_axis',(0.,0.,1.));
#10432=DIRECTION('ref_axis',(1.,0.,0.));
#10433=DIRECTION('center_axis',(0.,0.,1.));
#10434=DIRECTION('ref_axis',(1.,0.,0.));
#10435=DIRECTION('',(0.,0.,1.));
#10436=DIRECTION('center_axis',(0.,0.,-1.));
#10437=DIRECTION('ref_axis',(1.,0.,0.));
#10438=DIRECTION('center_axis',(0.,0.,1.));
#10439=DIRECTION('ref_axis',(1.,0.,0.));
#10440=DIRECTION('center_axis',(0.,0.,1.));
#10441=DIRECTION('ref_axis',(1.,0.,0.));
#10442=DIRECTION('center_axis',(0.,0.,-1.));
#10443=DIRECTION('ref_axis',(1.,0.,0.));
#10444=DIRECTION('',(0.,0.,1.));
#10445=DIRECTION('center_axis',(0.,0.,1.));
#10446=DIRECTION('ref_axis',(1.,0.,0.));
#10447=DIRECTION('center_axis',(0.,0.,1.));
#10448=DIRECTION('ref_axis',(1.,0.,0.));
#10449=DIRECTION('center_axis',(0.,0.,1.));
#10450=DIRECTION('ref_axis',(1.,0.,0.));
#10451=DIRECTION('center_axis',(0.,0.,1.));
#10452=DIRECTION('ref_axis',(1.,0.,0.));
#10453=DIRECTION('center_axis',(0.,0.,-1.));
#10454=DIRECTION('ref_axis',(1.,0.,0.));
#10455=DIRECTION('',(0.,0.,1.));
#10456=DIRECTION('center_axis',(0.,0.,1.));
#10457=DIRECTION('ref_axis',(1.,0.,0.));
#10458=DIRECTION('center_axis',(0.,0.,1.));
#10459=DIRECTION('ref_axis',(1.,0.,0.));
#10460=DIRECTION('center_axis',(0.,0.,1.));
#10461=DIRECTION('ref_axis',(1.,0.,0.));
#10462=DIRECTION('center_axis',(0.,0.,1.));
#10463=DIRECTION('ref_axis',(1.,0.,0.));
#10464=DIRECTION('center_axis',(0.,0.,-1.));
#10465=DIRECTION('ref_axis',(1.,0.,0.));
#10466=DIRECTION('',(0.,0.,1.));
#10467=DIRECTION('center_axis',(0.,0.,1.));
#10468=DIRECTION('ref_axis',(1.,0.,0.));
#10469=DIRECTION('center_axis',(0.,0.,1.));
#10470=DIRECTION('ref_axis',(1.,0.,0.));
#10471=DIRECTION('center_axis',(0.,0.,1.));
#10472=DIRECTION('ref_axis',(1.,0.,0.));
#10473=DIRECTION('center_axis',(0.,0.,1.));
#10474=DIRECTION('ref_axis',(1.,0.,0.));
#10475=DIRECTION('center_axis',(0.,0.,-1.));
#10476=DIRECTION('ref_axis',(1.,0.,0.));
#10477=DIRECTION('',(0.,0.,1.));
#10478=DIRECTION('center_axis',(0.,0.,1.));
#10479=DIRECTION('ref_axis',(1.,0.,0.));
#10480=DIRECTION('center_axis',(0.,0.,1.));
#10481=DIRECTION('ref_axis',(1.,0.,0.));
#10482=DIRECTION('center_axis',(0.,0.,1.));
#10483=DIRECTION('ref_axis',(1.,0.,0.));
#10484=DIRECTION('center_axis',(0.,0.,1.));
#10485=DIRECTION('ref_axis',(1.,0.,0.));
#10486=DIRECTION('center_axis',(0.,0.,1.));
#10487=DIRECTION('ref_axis',(1.,0.,0.));
#10488=DIRECTION('center_axis',(0.,0.,1.));
#10489=DIRECTION('ref_axis',(1.,0.,0.));
#10490=DIRECTION('center_axis',(0.,0.,1.));
#10491=DIRECTION('ref_axis',(1.,0.,0.));
#10492=DIRECTION('center_axis',(0.,0.,1.));
#10493=DIRECTION('ref_axis',(1.,0.,0.));
#10494=DIRECTION('center_axis',(0.,0.,-1.));
#10495=DIRECTION('ref_axis',(1.,0.,0.));
#10496=DIRECTION('center_axis',(0.,0.,1.));
#10497=DIRECTION('ref_axis',(1.,0.,0.));
#10498=DIRECTION('center_axis',(0.,0.,1.));
#10499=DIRECTION('ref_axis',(1.,0.,0.));
#10500=DIRECTION('',(0.,0.,1.));
#10501=DIRECTION('center_axis',(0.,0.,1.));
#10502=DIRECTION('ref_axis',(1.,0.,0.));
#10503=DIRECTION('center_axis',(0.,0.,1.));
#10504=DIRECTION('ref_axis',(1.,0.,0.));
#10505=DIRECTION('',(0.,0.,1.));
#10506=DIRECTION('center_axis',(0.,0.,1.));
#10507=DIRECTION('ref_axis',(1.,0.,0.));
#10508=DIRECTION('center_axis',(0.,0.,1.));
#10509=DIRECTION('ref_axis',(1.,0.,0.));
#10510=DIRECTION('',(0.,0.,1.));
#10511=DIRECTION('center_axis',(0.,0.,1.));
#10512=DIRECTION('ref_axis',(1.,0.,0.));
#10513=DIRECTION('center_axis',(0.,0.,1.));
#10514=DIRECTION('ref_axis',(1.,0.,0.));
#10515=DIRECTION('',(0.,0.,1.));
#10516=DIRECTION('center_axis',(0.,0.,1.));
#10517=DIRECTION('ref_axis',(1.,0.,0.));
#10518=DIRECTION('',(0.,0.,-1.));
#10519=DIRECTION('center_axis',(0.,0.,1.));
#10520=DIRECTION('ref_axis',(1.,0.,0.));
#10521=DIRECTION('center_axis',(0.,0.,1.));
#10522=DIRECTION('ref_axis',(1.,0.,0.));
#10523=DIRECTION('center_axis',(0.,0.,-1.));
#10524=DIRECTION('ref_axis',(1.,0.,0.));
#10525=DIRECTION('',(0.,0.,-1.));
#10526=DIRECTION('center_axis',(0.,0.,-1.));
#10527=DIRECTION('ref_axis',(1.,0.,0.));
#10528=DIRECTION('center_axis',(0.,0.,1.));
#10529=DIRECTION('ref_axis',(0.707106781186547,-0.707106781186548,0.));
#10530=DIRECTION('',(0.,0.,-1.));
#10531=DIRECTION('center_axis',(0.,0.,1.));
#10532=DIRECTION('ref_axis',(1.,0.,0.));
#10533=DIRECTION('center_axis',(0.,0.,1.));
#10534=DIRECTION('ref_axis',(1.,0.,0.));
#10535=DIRECTION('center_axis',(0.,0.,1.));
#10536=DIRECTION('ref_axis',(1.,0.,0.));
#10537=DIRECTION('axis',(0.,0.,1.));
#10538=DIRECTION('refdir',(1.,0.,0.));
#10539=DIRECTION('center_axis',(0.,0.,1.));
#10540=DIRECTION('ref_axis',(1.,0.,0.));
#10541=DIRECTION('center_axis',(0.,0.,1.));
#10542=DIRECTION('ref_axis',(1.,0.,0.));
#10543=DIRECTION('',(0.,0.,1.));
#10544=DIRECTION('center_axis',(0.,0.,-1.));
#10545=DIRECTION('ref_axis',(1.,0.,0.));
#10546=DIRECTION('center_axis',(0.,0.,1.));
#10547=DIRECTION('ref_axis',(1.,0.,0.));
#10548=DIRECTION('center_axis',(0.,0.,1.));
#10549=DIRECTION('ref_axis',(1.,0.,0.));
#10550=DIRECTION('',(0.,0.,1.));
#10551=DIRECTION('center_axis',(0.,0.,-1.));
#10552=DIRECTION('ref_axis',(1.,0.,0.));
#10553=DIRECTION('center_axis',(0.,0.,1.));
#10554=DIRECTION('ref_axis',(1.,0.,0.));
#10555=DIRECTION('center_axis',(0.,0.,1.));
#10556=DIRECTION('ref_axis',(1.,0.,0.));
#10557=DIRECTION('',(0.,0.,1.));
#10558=DIRECTION('center_axis',(0.,0.,-1.));
#10559=DIRECTION('ref_axis',(1.,0.,0.));
#10560=DIRECTION('center_axis',(0.,0.,1.));
#10561=DIRECTION('ref_axis',(1.,0.,0.));
#10562=DIRECTION('center_axis',(0.,0.,1.));
#10563=DIRECTION('ref_axis',(1.,0.,0.));
#10564=DIRECTION('',(0.,0.,1.));
#10565=DIRECTION('center_axis',(0.,0.,-1.));
#10566=DIRECTION('ref_axis',(1.,0.,0.));
#10567=DIRECTION('center_axis',(0.,0.,1.));
#10568=DIRECTION('ref_axis',(1.,0.,0.));
#10569=DIRECTION('center_axis',(0.,0.,1.));
#10570=DIRECTION('ref_axis',(1.,0.,0.));
#10571=DIRECTION('',(0.,0.,-1.));
#10572=DIRECTION('center_axis',(0.,0.,1.));
#10573=DIRECTION('ref_axis',(1.,0.,0.));
#10574=DIRECTION('center_axis',(0.,0.,1.));
#10575=DIRECTION('ref_axis',(1.,0.,0.));
#10576=DIRECTION('center_axis',(0.,0.,-1.));
#10577=DIRECTION('ref_axis',(1.,0.,0.));
#10578=DIRECTION('center_axis',(0.,0.,1.));
#10579=DIRECTION('ref_axis',(1.,0.,0.));
#10580=DIRECTION('center_axis',(0.,0.,-1.));
#10581=DIRECTION('ref_axis',(1.,0.,0.));
#10582=DIRECTION('',(0.,0.,-1.));
#10583=DIRECTION('center_axis',(0.,0.,1.));
#10584=DIRECTION('ref_axis',(1.,0.,0.));
#10585=DIRECTION('center_axis',(0.,0.,1.));
#10586=DIRECTION('ref_axis',(1.,0.,0.));
#10587=DIRECTION('',(0.,0.,-1.));
#10588=DIRECTION('center_axis',(0.,0.,1.));
#10589=DIRECTION('ref_axis',(1.,0.,0.));
#10590=DIRECTION('center_axis',(0.,0.,1.));
#10591=DIRECTION('ref_axis',(1.,0.,0.));
#10592=DIRECTION('center_axis',(0.,0.,1.));
#10593=DIRECTION('ref_axis',(1.,0.,0.));
#10594=DIRECTION('axis',(0.,0.,1.));
#10595=DIRECTION('refdir',(1.,0.,0.));
#10596=DIRECTION('center_axis',(0.866025403784439,0.,-0.5));
#10597=DIRECTION('ref_axis',(0.5,0.,0.866025403784439));
#10598=DIRECTION('',(-0.5,0.,-0.866025403784439));
#10599=DIRECTION('',(0.,-1.,0.));
#10600=DIRECTION('',(0.5,0.,0.866025403784439));
#10601=DIRECTION('',(0.,-1.,0.));
#10602=DIRECTION('center_axis',(1.92296268638356E-16,0.,-1.));
#10603=DIRECTION('ref_axis',(1.,0.,1.92296268638356E-16));
#10604=DIRECTION('',(-1.,0.,-1.92296268638356E-16));
#10605=DIRECTION('',(0.,-1.,0.));
#10606=DIRECTION('',(1.,0.,1.92296268638356E-16));
#10607=DIRECTION('center_axis',(-0.866025403784439,0.,-0.5));
#10608=DIRECTION('ref_axis',(0.5,0.,-0.866025403784439));
#10609=DIRECTION('',(-0.5,0.,0.866025403784438));
#10610=DIRECTION('',(0.,-1.,0.));
#10611=DIRECTION('',(0.5,0.,-0.866025403784438));
#10612=DIRECTION('center_axis',(-0.866025403784439,0.,0.5));
#10613=DIRECTION('ref_axis',(-0.5,0.,-0.866025403784439));
#10614=DIRECTION('',(0.5,0.,0.866025403784439));
#10615=DIRECTION('',(0.,-1.,0.));
#10616=DIRECTION('',(-0.5,0.,-0.866025403784439));
#10617=DIRECTION('center_axis',(-1.92296268638356E-16,0.,1.));
#10618=DIRECTION('ref_axis',(-1.,0.,-1.92296268638356E-16));
#10619=DIRECTION('',(1.,0.,1.92296268638356E-16));
#10620=DIRECTION('',(0.,-1.,0.));
#10621=DIRECTION('',(-1.,0.,-1.92296268638356E-16));
#10622=DIRECTION('center_axis',(0.866025403784439,0.,0.5));
#10623=DIRECTION('ref_axis',(-0.5,0.,0.866025403784439));
#10624=DIRECTION('',(0.5,0.,-0.866025403784439));
#10625=DIRECTION('',(-0.5,0.,0.866025403784439));
#10626=DIRECTION('center_axis',(0.,1.,0.));
#10627=DIRECTION('ref_axis',(1.,0.,0.));
#10628=DIRECTION('center_axis',(0.,-1.,0.));
#10629=DIRECTION('ref_axis',(0.,0.,-1.));
#10630=DIRECTION('center_axis',(0.,1.,0.));
#10631=DIRECTION('ref_axis',(1.,0.,0.));
#10632=DIRECTION('center_axis',(0.,1.,0.));
#10633=DIRECTION('ref_axis',(1.,0.,0.));
#10634=DIRECTION('center_axis',(0.,1.,0.));
#10635=DIRECTION('ref_axis',(0.,0.,1.));
#10636=DIRECTION('center_axis',(0.,-1.,0.));
#10637=DIRECTION('ref_axis',(1.,0.,0.));
#10638=DIRECTION('center_axis',(0.,-1.,0.));
#10639=DIRECTION('ref_axis',(1.,0.,0.));
#10640=DIRECTION('center_axis',(0.,-1.,0.));
#10641=DIRECTION('ref_axis',(1.,0.,0.));
#10642=DIRECTION('',(0.707106781186548,0.707106781186547,8.65956056235494E-17));
#10643=DIRECTION('center_axis',(0.,-1.,0.));
#10644=DIRECTION('ref_axis',(1.,0.,0.));
#10645=DIRECTION('center_axis',(0.,-1.,0.));
#10646=DIRECTION('ref_axis',(1.,0.,0.));
#10647=DIRECTION('',(0.,1.,0.));
#10648=DIRECTION('center_axis',(0.,1.,0.));
#10649=DIRECTION('ref_axis',(1.,0.,0.));
#10650=DIRECTION('center_axis',(0.,-1.,0.));
#10651=DIRECTION('ref_axis',(1.,0.,0.));
#10652=DIRECTION('',(-0.707106781186547,0.707106781186548,-8.65956056235493E-17));
#10653=DIRECTION('center_axis',(0.,-1.,0.));
#10654=DIRECTION('ref_axis',(0.,0.,-1.));
#10655=DIRECTION('center_axis',(0.,-1.,0.));
#10656=DIRECTION('ref_axis',(1.,0.,0.));
#10657=DIRECTION('center_axis',(0.,1.,0.));
#10658=DIRECTION('ref_axis',(1.,0.,0.));
#10659=DIRECTION('center_axis',(0.,1.,0.));
#10660=DIRECTION('ref_axis',(1.,0.,0.));
#10661=DIRECTION('',(-0.447213595499958,0.894427190999916,-5.47678698264203E-17));
#10662=DIRECTION('center_axis',(0.,-1.,0.));
#10663=DIRECTION('ref_axis',(1.,0.,0.));
#10664=DIRECTION('',(0.,1.,0.));
#10665=DIRECTION('axis',(0.,0.,1.));
#10666=DIRECTION('refdir',(1.,0.,0.));
#10667=DIRECTION('axis',(0.,0.,1.));
#10668=DIRECTION('refdir',(1.,0.,0.));
#10669=DIRECTION('center_axis',(0.,-1.,0.));
#10670=DIRECTION('ref_axis',(0.,0.,-1.));
#10671=DIRECTION('center_axis',(0.,-1.,0.));
#10672=DIRECTION('ref_axis',(1.,0.,0.));
#10673=DIRECTION('center_axis',(0.,-1.,0.));
#10674=DIRECTION('ref_axis',(1.,0.,0.));
#10675=DIRECTION('center_axis',(1.,0.,1.22464679914735E-16));
#10676=DIRECTION('ref_axis',(-1.22464679914735E-16,0.,1.));
#10677=DIRECTION('center_axis',(0.,1.,0.));
#10678=DIRECTION('ref_axis',(1.,0.,0.));
#10679=DIRECTION('center_axis',(0.,1.,0.));
#10680=DIRECTION('ref_axis',(1.,0.,0.));
#10681=DIRECTION('center_axis',(0.,-1.,0.));
#10682=DIRECTION('ref_axis',(1.,0.,0.));
#10683=DIRECTION('',(0.,1.,0.));
#10684=DIRECTION('center_axis',(0.,-1.,0.));
#10685=DIRECTION('ref_axis',(1.,0.,0.));
#10686=DIRECTION('center_axis',(0.,-1.,0.));
#10687=DIRECTION('ref_axis',(1.,0.,0.));
#10688=DIRECTION('center_axis',(0.,-1.,0.));
#10689=DIRECTION('ref_axis',(1.,0.,0.));
#10690=DIRECTION('',(0.,1.,0.));
#10691=DIRECTION('center_axis',(0.,-1.,0.));
#10692=DIRECTION('ref_axis',(1.,0.,0.));
#10693=DIRECTION('center_axis',(0.,1.,0.));
#10694=DIRECTION('ref_axis',(1.,0.,0.));
#10695=DIRECTION('',(-0.707106781186548,0.707106781186547,-8.65956056235494E-17));
#10696=DIRECTION('center_axis',(0.,-1.,0.));
#10697=DIRECTION('ref_axis',(1.,0.,0.));
#10698=DIRECTION('center_axis',(0.,1.,0.));
#10699=DIRECTION('ref_axis',(0.,0.,1.));
#10700=DIRECTION('center_axis',(0.,-1.,0.));
#10701=DIRECTION('ref_axis',(1.,0.,0.));
#10702=DIRECTION('center_axis',(0.,-1.,0.));
#10703=DIRECTION('ref_axis',(1.,0.,0.));
#10704=DIRECTION('',(0.,1.,0.));
#10705=DIRECTION('center_axis',(0.,-1.,0.));
#10706=DIRECTION('ref_axis',(0.,0.,-1.));
#10707=DIRECTION('center_axis',(0.,-1.,0.));
#10708=DIRECTION('ref_axis',(1.,0.,0.));
#10709=DIRECTION('center_axis',(0.,-1.,0.));
#10710=DIRECTION('ref_axis',(1.,0.,0.));
#10711=DIRECTION('',(0.707106781186548,0.707106781186547,8.65956056235494E-17));
#10712=DIRECTION('axis',(0.,0.,1.));
#10713=DIRECTION('refdir',(1.,0.,0.));
#10714=DIRECTION('center_axis',(0.,-1.,0.));
#10715=DIRECTION('ref_axis',(0.,0.,-1.));
#10716=DIRECTION('center_axis',(0.,-1.,0.));
#10717=DIRECTION('ref_axis',(1.,0.,0.));
#10718=DIRECTION('center_axis',(0.,-1.,0.));
#10719=DIRECTION('ref_axis',(1.,0.,0.));
#10720=DIRECTION('center_axis',(1.,0.,1.22464679914735E-16));
#10721=DIRECTION('ref_axis',(-1.22464679914735E-16,0.,1.));
#10722=DIRECTION('center_axis',(0.,1.,0.));
#10723=DIRECTION('ref_axis',(1.,0.,0.));
#10724=DIRECTION('center_axis',(0.,1.,0.));
#10725=DIRECTION('ref_axis',(1.,0.,0.));
#10726=DIRECTION('center_axis',(0.,-1.,0.));
#10727=DIRECTION('ref_axis',(1.,0.,0.));
#10728=DIRECTION('center_axis',(0.,-1.,0.));
#10729=DIRECTION('ref_axis',(1.,0.,0.));
#10730=DIRECTION('',(0.,1.,0.));
#10731=DIRECTION('center_axis',(0.,1.,0.));
#10732=DIRECTION('ref_axis',(0.,0.,1.));
#10733=DIRECTION('center_axis',(0.,-1.,0.));
#10734=DIRECTION('ref_axis',(1.,0.,0.));
#10735=DIRECTION('center_axis',(0.,-1.,0.));
#10736=DIRECTION('ref_axis',(1.,0.,0.));
#10737=DIRECTION('center_axis',(0.,-1.,0.));
#10738=DIRECTION('ref_axis',(1.,0.,0.));
#10739=DIRECTION('center_axis',(0.,-1.,0.));
#10740=DIRECTION('ref_axis',(1.,0.,0.));
#10741=DIRECTION('',(0.707106781186548,0.707106781186547,8.65956056235494E-17));
#10742=DIRECTION('center_axis',(0.,-1.,0.));
#10743=DIRECTION('ref_axis',(1.,0.,0.));
#10744=DIRECTION('center_axis',(0.,-1.,0.));
#10745=DIRECTION('ref_axis',(1.,0.,0.));
#10746=DIRECTION('',(0.,1.,0.));
#10747=DIRECTION('center_axis',(0.,1.,0.));
#10748=DIRECTION('ref_axis',(1.,0.,0.));
#10749=DIRECTION('center_axis',(0.,-1.,0.));
#10750=DIRECTION('ref_axis',(1.,0.,0.));
#10751=DIRECTION('',(-0.707106781186548,0.707106781186547,-8.65956056235494E-17));
#10752=DIRECTION('center_axis',(0.,-1.,0.));
#10753=DIRECTION('ref_axis',(0.,0.,-1.));
#10754=DIRECTION('center_axis',(0.,-1.,0.));
#10755=DIRECTION('ref_axis',(1.,0.,0.));
#10756=DIRECTION('',(0.,1.,0.));
#10757=DIRECTION('axis',(0.,0.,1.));
#10758=DIRECTION('refdir',(1.,0.,0.));
#10759=DIRECTION('center_axis',(0.,0.,1.));
#10760=DIRECTION('ref_axis',(1.,0.,0.));
#10761=DIRECTION('center_axis',(1.22464679914735E-16,-1.,0.));
#10762=DIRECTION('ref_axis',(-1.,-1.22464679914735E-16,0.));
#10763=DIRECTION('center_axis',(0.642787609686539,0.,0.766044443118978));
#10764=DIRECTION('ref_axis',(0.766044443118978,0.,-0.642787609686539));
#10765=DIRECTION('center_axis',(9.38133875270273E-17,-1.,-7.87187788734199E-17));
#10766=DIRECTION('ref_axis',(-0.766044443118978,-1.22464679914735E-16,0.642787609686539));
#10767=DIRECTION('center_axis',(0.984807753012208,0.,0.173648177666931));
#10768=DIRECTION('ref_axis',(0.17364817766693,0.,-0.984807753012208));
#10769=DIRECTION('center_axis',(2.12657684957577E-17,-1.,-1.2060416625019E-16));
#10770=DIRECTION('ref_axis',(-0.17364817766693,-1.22464679914735E-16,0.984807753012208));
#10771=DIRECTION('center_axis',(0.866025403784439,0.,-0.5));
#10772=DIRECTION('ref_axis',(-0.5,0.,-0.866025403784439));
#10773=DIRECTION('center_axis',(-6.12323399573676E-17,-1.,-1.06057523872491E-16));
#10774=DIRECTION('ref_axis',(0.5,-1.22464679914735E-16,0.866025403784439));
#10775=DIRECTION('center_axis',(0.342020143325669,0.,-0.939692620785908));
#10776=DIRECTION('ref_axis',(-0.939692620785908,0.,-0.342020143325669));
#10777=DIRECTION('center_axis',(-1.15079156022785E-16,-1.,-4.18853873767699E-17));
#10778=DIRECTION('ref_axis',(0.939692620785908,-1.22464679914735E-16,0.342020143325669));
#10779=DIRECTION('center_axis',(-0.342020143325669,0.,-0.939692620785908));
#10780=DIRECTION('ref_axis',(-0.939692620785909,0.,0.342020143325669));
#10781=DIRECTION('center_axis',(-1.15079156022785E-16,-1.,4.18853873767699E-17));
#10782=DIRECTION('ref_axis',(0.939692620785908,-1.22464679914735E-16,-0.342020143325669));
#10783=DIRECTION('center_axis',(-0.866025403784438,0.,-0.5));
#10784=DIRECTION('ref_axis',(-0.5,0.,0.866025403784438));
#10785=DIRECTION('center_axis',(-6.12323399573677E-17,-1.,1.06057523872491E-16));
#10786=DIRECTION('ref_axis',(0.5,-1.22464679914735E-16,-0.866025403784438));
#10787=DIRECTION('center_axis',(-0.984807753012208,0.,0.17364817766693));
#10788=DIRECTION('ref_axis',(0.17364817766693,0.,0.984807753012208));
#10789=DIRECTION('center_axis',(2.12657684957577E-17,-1.,1.2060416625019E-16));
#10790=DIRECTION('ref_axis',(-0.17364817766693,-1.22464679914735E-16,-0.984807753012208));
#10791=DIRECTION('center_axis',(-0.64278760968654,0.,0.766044443118978));
#10792=DIRECTION('ref_axis',(0.766044443118978,0.,0.64278760968654));
#10793=DIRECTION('center_axis',(9.38133875270273E-17,-1.,7.87187788734199E-17));
#10794=DIRECTION('ref_axis',(-0.766044443118978,-1.22464679914735E-16,-0.64278760968654));
#10795=DIRECTION('axis',(0.,0.,1.));
#10796=DIRECTION('refdir',(1.,0.,0.));
#10797=DIRECTION('center_axis',(0.,0.,1.));
#10798=DIRECTION('ref_axis',(1.,0.,0.));
#10799=DIRECTION('center_axis',(0.,-1.,0.));
#10800=DIRECTION('ref_axis',(0.,0.,-1.));
#10801=DIRECTION('center_axis',(0.,-1.,0.));
#10802=DIRECTION('ref_axis',(0.,0.,-1.));
#10803=DIRECTION('center_axis',(0.,1.,0.));
#10804=DIRECTION('ref_axis',(1.,0.,0.));
#10805=DIRECTION('center_axis',(0.,1.,0.));
#10806=DIRECTION('ref_axis',(1.,0.,0.));
#10807=DIRECTION('center_axis',(0.,1.,0.));
#10808=DIRECTION('ref_axis',(1.,0.,0.));
#10809=DIRECTION('center_axis',(0.,1.,0.));
#10810=DIRECTION('ref_axis',(1.,0.,0.));
#10811=DIRECTION('center_axis',(0.,1.,0.));
#10812=DIRECTION('ref_axis',(1.,0.,0.));
#10813=DIRECTION('',(0.,-1.,0.));
#10814=DIRECTION('center_axis',(0.,-1.,0.));
#10815=DIRECTION('ref_axis',(1.,0.,0.));
#10816=DIRECTION('center_axis',(0.,1.,0.));
#10817=DIRECTION('ref_axis',(1.,0.,0.));
#10818=DIRECTION('center_axis',(0.,1.,0.));
#10819=DIRECTION('ref_axis',(1.,0.,0.));
#10820=DIRECTION('center_axis',(0.,1.,0.));
#10821=DIRECTION('ref_axis',(1.,0.,0.));
#10822=DIRECTION('center_axis',(0.,1.,0.));
#10823=DIRECTION('ref_axis',(1.,0.,0.));
#10824=DIRECTION('center_axis',(0.,1.,0.));
#10825=DIRECTION('ref_axis',(1.,0.,0.));
#10826=DIRECTION('center_axis',(0.,1.,0.));
#10827=DIRECTION('ref_axis',(1.,0.,0.));
#10828=DIRECTION('center_axis',(0.,1.,0.));
#10829=DIRECTION('ref_axis',(1.,0.,0.));
#10830=DIRECTION('center_axis',(0.,-1.,0.));
#10831=DIRECTION('ref_axis',(1.,0.,0.));
#10832=DIRECTION('center_axis',(0.,-1.,0.));
#10833=DIRECTION('ref_axis',(0.,0.,-1.));
#10834=DIRECTION('center_axis',(0.,0.,1.));
#10835=DIRECTION('ref_axis',(1.,0.,0.));
#10836=DIRECTION('center_axis',(0.,-1.,0.));
#10837=DIRECTION('ref_axis',(0.,0.,-1.));
#10838=DIRECTION('center_axis',(0.,1.,0.));
#10839=DIRECTION('ref_axis',(1.,0.,0.));
#10840=DIRECTION('center_axis',(0.,-1.,0.));
#10841=DIRECTION('ref_axis',(1.,0.,0.));
#10842=DIRECTION('center_axis',(0.,-1.,0.));
#10843=DIRECTION('ref_axis',(0.,0.,-1.));
#10844=DIRECTION('center_axis',(0.,0.,1.));
#10845=DIRECTION('ref_axis',(1.,0.,0.));
#10846=DIRECTION('center_axis',(0.,-1.,0.));
#10847=DIRECTION('ref_axis',(0.,0.,-1.));
#10848=DIRECTION('center_axis',(0.,1.,0.));
#10849=DIRECTION('ref_axis',(1.,0.,0.));
#10850=DIRECTION('center_axis',(0.,-1.,0.));
#10851=DIRECTION('ref_axis',(1.,0.,0.));
#10852=DIRECTION('center_axis',(0.,-1.,0.));
#10853=DIRECTION('ref_axis',(0.,0.,-1.));
#10854=DIRECTION('center_axis',(0.,0.,1.));
#10855=DIRECTION('ref_axis',(1.,0.,0.));
#10856=DIRECTION('center_axis',(0.,-1.,0.));
#10857=DIRECTION('ref_axis',(0.,0.,-1.));
#10858=DIRECTION('center_axis',(0.,1.,0.));
#10859=DIRECTION('ref_axis',(1.,0.,0.));
#10860=DIRECTION('center_axis',(0.,-1.,0.));
#10861=DIRECTION('ref_axis',(1.,0.,0.));
#10862=DIRECTION('center_axis',(0.,-1.,0.));
#10863=DIRECTION('ref_axis',(1.,0.,0.));
#10864=DIRECTION('center_axis',(0.,-1.,0.));
#10865=DIRECTION('ref_axis',(0.,0.,-1.));
#10866=DIRECTION('center_axis',(0.,0.,1.));
#10867=DIRECTION('ref_axis',(1.,0.,0.));
#10868=DIRECTION('center_axis',(0.,-1.,0.));
#10869=DIRECTION('ref_axis',(0.,0.,-1.));
#10870=DIRECTION('center_axis',(0.,1.,0.));
#10871=DIRECTION('ref_axis',(1.,0.,0.));
#10872=DIRECTION('center_axis',(0.,-1.,0.));
#10873=DIRECTION('ref_axis',(1.,0.,0.));
#10874=DIRECTION('center_axis',(0.,-1.,0.));
#10875=DIRECTION('ref_axis',(0.,0.,-1.));
#10876=DIRECTION('center_axis',(0.,0.,1.));
#10877=DIRECTION('ref_axis',(1.,0.,0.));
#10878=DIRECTION('center_axis',(0.,-1.,0.));
#10879=DIRECTION('ref_axis',(0.,0.,-1.));
#10880=DIRECTION('center_axis',(0.,1.,0.));
#10881=DIRECTION('ref_axis',(1.,0.,0.));
#10882=DIRECTION('center_axis',(0.,-1.,0.));
#10883=DIRECTION('ref_axis',(1.,0.,0.));
#10884=DIRECTION('center_axis',(0.,-1.,0.));
#10885=DIRECTION('ref_axis',(0.,0.,-1.));
#10886=DIRECTION('center_axis',(0.,0.,1.));
#10887=DIRECTION('ref_axis',(1.,0.,0.));
#10888=DIRECTION('center_axis',(0.,-1.,0.));
#10889=DIRECTION('ref_axis',(0.,0.,-1.));
#10890=DIRECTION('center_axis',(0.,1.,0.));
#10891=DIRECTION('ref_axis',(1.,0.,0.));
#10892=DIRECTION('center_axis',(0.,-1.,0.));
#10893=DIRECTION('ref_axis',(1.,0.,0.));
#10894=DIRECTION('center_axis',(0.,-1.,0.));
#10895=DIRECTION('ref_axis',(0.,0.,-1.));
#10896=DIRECTION('center_axis',(0.,0.,1.));
#10897=DIRECTION('ref_axis',(1.,0.,0.));
#10898=DIRECTION('center_axis',(0.,-1.,0.));
#10899=DIRECTION('ref_axis',(0.,0.,-1.));
#10900=DIRECTION('center_axis',(0.,1.,0.));
#10901=DIRECTION('ref_axis',(1.,0.,0.));
#10902=DIRECTION('center_axis',(0.,1.,0.));
#10903=DIRECTION('ref_axis',(1.,0.,0.));
#10904=DIRECTION('',(0.,1.,0.));
#10905=DIRECTION('center_axis',(0.,-1.,0.));
#10906=DIRECTION('ref_axis',(1.,0.,0.));
#10907=DIRECTION('center_axis',(0.,-1.,0.));
#10908=DIRECTION('ref_axis',(1.,0.,0.));
#10909=DIRECTION('center_axis',(0.,1.,0.));
#10910=DIRECTION('ref_axis',(1.,0.,0.));
#10911=DIRECTION('center_axis',(0.,-1.,0.));
#10912=DIRECTION('ref_axis',(0.,0.,-1.));
#10913=DIRECTION('center_axis',(0.,0.,1.));
#10914=DIRECTION('ref_axis',(1.,0.,0.));
#10915=DIRECTION('center_axis',(0.,-1.,0.));
#10916=DIRECTION('ref_axis',(0.,0.,-1.));
#10917=DIRECTION('center_axis',(0.,-1.,0.));
#10918=DIRECTION('ref_axis',(-1.,0.,0.));
#10919=DIRECTION('center_axis',(0.,1.,0.));
#10920=DIRECTION('ref_axis',(1.,0.,0.));
#10921=DIRECTION('axis',(0.,0.,1.));
#10922=DIRECTION('refdir',(1.,0.,0.));
#10923=DIRECTION('center_axis',(0.,1.,0.));
#10924=DIRECTION('ref_axis',(0.,0.,1.));
#10925=DIRECTION('center_axis',(0.,-1.,0.));
#10926=DIRECTION('ref_axis',(1.,0.,0.));
#10927=DIRECTION('center_axis',(0.,-1.,0.));
#10928=DIRECTION('ref_axis',(1.,0.,0.));
#10929=DIRECTION('center_axis',(0.,-1.,0.));
#10930=DIRECTION('ref_axis',(1.,0.,0.));
#10931=DIRECTION('center_axis',(0.,-1.,0.));
#10932=DIRECTION('ref_axis',(1.,0.,0.));
#10933=DIRECTION('',(0.,1.,0.));
#10934=DIRECTION('center_axis',(0.,-1.,0.));
#10935=DIRECTION('ref_axis',(0.,0.,-1.));
#10936=DIRECTION('center_axis',(0.,-1.,0.));
#10937=DIRECTION('ref_axis',(1.,0.,0.));
#10938=DIRECTION('center_axis',(0.,-1.,0.));
#10939=DIRECTION('ref_axis',(1.,0.,0.));
#10940=DIRECTION('',(0.,1.,0.));
#10941=DIRECTION('center_axis',(0.,1.,0.));
#10942=DIRECTION('ref_axis',(0.,0.,1.));
#10943=DIRECTION('center_axis',(0.,-1.,0.));
#10944=DIRECTION('ref_axis',(1.,0.,0.));
#10945=DIRECTION('center_axis',(0.,-1.,0.));
#10946=DIRECTION('ref_axis',(1.,0.,0.));
#10947=DIRECTION('center_axis',(0.,-1.,0.));
#10948=DIRECTION('ref_axis',(1.,0.,0.));
#10949=DIRECTION('center_axis',(0.,-1.,0.));
#10950=DIRECTION('ref_axis',(1.,0.,0.));
#10951=DIRECTION('',(0.,1.,0.));
#10952=DIRECTION('center_axis',(0.,-1.,0.));
#10953=DIRECTION('ref_axis',(0.,0.,-1.));
#10954=DIRECTION('center_axis',(0.,-1.,0.));
#10955=DIRECTION('ref_axis',(1.,0.,0.));
#10956=DIRECTION('center_axis',(0.,-1.,0.));
#10957=DIRECTION('ref_axis',(1.,0.,0.));
#10958=DIRECTION('',(0.,1.,0.));
#10959=DIRECTION('',(0.,0.,1.));
#10960=DIRECTION('',(1.,0.,0.));
#10961=DIRECTION('',(0.,0.,1.));
#10962=DIRECTION('',(1.,0.,0.));
#10963=DIRECTION('',(0.,0.,1.));
#10964=DIRECTION('',(1.,0.,0.));
#10965=DIRECTION('',(0.,0.,1.));
#10966=DIRECTION('',(1.,0.,0.));
#10967=DIRECTION('',(0.,0.,1.));
#10968=DIRECTION('',(1.,0.,0.));
#10969=DIRECTION('axis',(0.,0.,1.));
#10970=DIRECTION('refdir',(1.,0.,0.));
#10971=DIRECTION('center_axis',(0.,1.,0.));
#10972=DIRECTION('ref_axis',(-1.,0.,0.));
#10973=DIRECTION('',(-1.,0.,0.));
#10974=DIRECTION('',(0.,0.,1.));
#10975=DIRECTION('',(-1.,0.,0.));
#10976=DIRECTION('',(0.,0.,1.));
#10977=DIRECTION('center_axis',(1.,0.,0.));
#10978=DIRECTION('ref_axis',(0.,1.,0.));
#10979=DIRECTION('',(0.,1.,0.));
#10980=DIRECTION('',(0.,1.,0.));
#10981=DIRECTION('',(0.,0.,1.));
#10982=DIRECTION('center_axis',(0.,-1.,0.));
#10983=DIRECTION('ref_axis',(1.,0.,0.));
#10984=DIRECTION('',(1.,0.,0.));
#10985=DIRECTION('',(1.,0.,0.));
#10986=DIRECTION('',(0.,0.,1.));
#10987=DIRECTION('center_axis',(-1.,0.,0.));
#10988=DIRECTION('ref_axis',(0.,-1.,0.));
#10989=DIRECTION('',(0.,-1.,0.));
#10990=DIRECTION('',(0.,-1.,0.));
#10991=DIRECTION('center_axis',(0.,0.,1.));
#10992=DIRECTION('ref_axis',(1.,0.,0.));
#10993=DIRECTION('center_axis',(0.,0.,1.));
#10994=DIRECTION('ref_axis',(1.,0.,0.));
#10995=DIRECTION('axis',(0.,0.,1.));
#10996=DIRECTION('refdir',(1.,0.,0.));
#10997=DIRECTION('center_axis',(0.,1.,0.));
#10998=DIRECTION('ref_axis',(-1.,0.,0.));
#10999=DIRECTION('',(-1.,0.,0.));
#11000=DIRECTION('',(0.,0.,1.));
#11001=DIRECTION('',(-1.,0.,0.));
#11002=DIRECTION('',(0.,0.,1.));
#11003=DIRECTION('center_axis',(1.,0.,0.));
#11004=DIRECTION('ref_axis',(0.,1.,0.));
#11005=DIRECTION('',(0.,1.,0.));
#11006=DIRECTION('',(0.,1.,0.));
#11007=DIRECTION('',(0.,0.,1.));
#11008=DIRECTION('center_axis',(0.,-1.,0.));
#11009=DIRECTION('ref_axis',(1.,0.,0.));
#11010=DIRECTION('',(1.,0.,0.));
#11011=DIRECTION('',(1.,0.,0.));
#11012=DIRECTION('',(0.,0.,1.));
#11013=DIRECTION('center_axis',(-1.,0.,0.));
#11014=DIRECTION('ref_axis',(0.,-1.,0.));
#11015=DIRECTION('',(0.,-1.,0.));
#11016=DIRECTION('',(0.,-1.,0.));
#11017=DIRECTION('center_axis',(0.,0.,1.));
#11018=DIRECTION('ref_axis',(1.,0.,0.));
#11019=DIRECTION('center_axis',(0.,0.,1.));
#11020=DIRECTION('ref_axis',(1.,0.,0.));
#11021=DIRECTION('axis',(0.,0.,1.));
#11022=DIRECTION('refdir',(1.,0.,0.));
#11023=DIRECTION('axis',(0.,0.,1.));
#11024=DIRECTION('refdir',(1.,0.,0.));
#11025=DIRECTION('center_axis',(0.,0.,1.));
#11026=DIRECTION('ref_axis',(1.,0.,0.));
#11027=DIRECTION('center_axis',(0.,0.,1.));
#11028=DIRECTION('ref_axis',(1.,0.,0.));
#11029=DIRECTION('',(0.,0.,1.));
#11030=DIRECTION('center_axis',(0.,0.,-1.));
#11031=DIRECTION('ref_axis',(1.,0.,0.));
#11032=DIRECTION('center_axis',(0.,0.,1.));
#11033=DIRECTION('ref_axis',(1.,0.,0.));
#11034=DIRECTION('center_axis',(0.,0.,1.));
#11035=DIRECTION('ref_axis',(1.,0.,0.));
#11036=DIRECTION('center_axis',(0.,0.,1.));
#11037=DIRECTION('ref_axis',(1.,0.,0.));
#11038=DIRECTION('',(0.,0.,1.));
#11039=DIRECTION('center_axis',(0.,0.,-1.));
#11040=DIRECTION('ref_axis',(1.,0.,0.));
#11041=DIRECTION('center_axis',(0.,0.,1.));
#11042=DIRECTION('ref_axis',(1.,0.,0.));
#11043=DIRECTION('center_axis',(0.,0.,1.));
#11044=DIRECTION('ref_axis',(1.,0.,0.));
#11045=DIRECTION('center_axis',(0.,0.,1.));
#11046=DIRECTION('ref_axis',(1.,0.,0.));
#11047=DIRECTION('',(0.,0.,1.));
#11048=DIRECTION('center_axis',(0.,0.,-1.));
#11049=DIRECTION('ref_axis',(1.,0.,0.));
#11050=DIRECTION('center_axis',(0.,0.,1.));
#11051=DIRECTION('ref_axis',(1.,0.,0.));
#11052=DIRECTION('center_axis',(0.,0.,1.));
#11053=DIRECTION('ref_axis',(1.,0.,0.));
#11054=DIRECTION('center_axis',(0.,0.,1.));
#11055=DIRECTION('ref_axis',(1.,0.,0.));
#11056=DIRECTION('center_axis',(0.,0.,-1.));
#11057=DIRECTION('ref_axis',(1.,0.,0.));
#11058=DIRECTION('center_axis',(0.,0.,1.));
#11059=DIRECTION('ref_axis',(1.,0.,0.));
#11060=DIRECTION('center_axis',(0.,0.,1.));
#11061=DIRECTION('ref_axis',(1.,0.,0.));
#11062=DIRECTION('',(0.,0.,-1.));
#11063=DIRECTION('center_axis',(0.,0.,1.));
#11064=DIRECTION('ref_axis',(1.,0.,0.));
#11065=DIRECTION('',(0.,0.,-1.));
#11066=DIRECTION('center_axis',(0.,0.,1.));
#11067=DIRECTION('ref_axis',(1.,0.,0.));
#11068=DIRECTION('center_axis',(0.,0.,1.));
#11069=DIRECTION('ref_axis',(1.,0.,0.));
#11070=DIRECTION('center_axis',(0.,0.,1.));
#11071=DIRECTION('ref_axis',(1.,0.,0.));
#11072=DIRECTION('axis',(0.,0.,1.));
#11073=DIRECTION('refdir',(1.,0.,0.));
#11074=DIRECTION('center_axis',(0.,0.,1.));
#11075=DIRECTION('ref_axis',(1.,0.,0.));
#11076=DIRECTION('center_axis',(0.,0.,1.));
#11077=DIRECTION('ref_axis',(1.,0.,0.));
#11078=DIRECTION('',(0.,0.,1.));
#11079=DIRECTION('center_axis',(0.,0.,-1.));
#11080=DIRECTION('ref_axis',(1.,0.,0.));
#11081=DIRECTION('center_axis',(0.,0.,1.));
#11082=DIRECTION('ref_axis',(1.,0.,0.));
#11083=DIRECTION('center_axis',(0.,0.,1.));
#11084=DIRECTION('ref_axis',(1.,0.,0.));
#11085=DIRECTION('',(0.,0.,1.));
#11086=DIRECTION('center_axis',(0.,0.,-1.));
#11087=DIRECTION('ref_axis',(1.,0.,0.));
#11088=DIRECTION('center_axis',(0.,0.,1.));
#11089=DIRECTION('ref_axis',(1.,0.,0.));
#11090=DIRECTION('center_axis',(0.,0.,1.));
#11091=DIRECTION('ref_axis',(1.,0.,0.));
#11092=DIRECTION('',(0.,0.,1.));
#11093=DIRECTION('center_axis',(0.,0.,-1.));
#11094=DIRECTION('ref_axis',(1.,0.,0.));
#11095=DIRECTION('center_axis',(0.,0.,1.));
#11096=DIRECTION('ref_axis',(1.,0.,0.));
#11097=DIRECTION('center_axis',(0.,0.,1.));
#11098=DIRECTION('ref_axis',(1.,0.,0.));
#11099=DIRECTION('',(0.,0.,1.));
#11100=DIRECTION('center_axis',(0.,0.,-1.));
#11101=DIRECTION('ref_axis',(1.,0.,0.));
#11102=DIRECTION('center_axis',(0.,0.,1.));
#11103=DIRECTION('ref_axis',(1.,0.,0.));
#11104=DIRECTION('center_axis',(0.,0.,1.));
#11105=DIRECTION('ref_axis',(1.,0.,0.));
#11106=DIRECTION('',(0.,0.,1.));
#11107=DIRECTION('center_axis',(0.,0.,-1.));
#11108=DIRECTION('ref_axis',(1.,0.,0.));
#11109=DIRECTION('center_axis',(0.,0.,1.));
#11110=DIRECTION('ref_axis',(1.,0.,0.));
#11111=DIRECTION('center_axis',(0.,0.,1.));
#11112=DIRECTION('ref_axis',(1.,0.,0.));
#11113=DIRECTION('',(0.,0.,1.));
#11114=DIRECTION('center_axis',(0.,0.,-1.));
#11115=DIRECTION('ref_axis',(1.,0.,0.));
#11116=DIRECTION('center_axis',(0.,0.,1.));
#11117=DIRECTION('ref_axis',(1.,0.,0.));
#11118=DIRECTION('center_axis',(0.,0.,1.));
#11119=DIRECTION('ref_axis',(1.,0.,0.));
#11120=DIRECTION('',(0.,0.,1.));
#11121=DIRECTION('center_axis',(0.,0.,-1.));
#11122=DIRECTION('ref_axis',(1.,0.,0.));
#11123=DIRECTION('center_axis',(0.,0.,1.));
#11124=DIRECTION('ref_axis',(1.,0.,0.));
#11125=DIRECTION('center_axis',(0.,0.,1.));
#11126=DIRECTION('ref_axis',(1.,0.,0.));
#11127=DIRECTION('',(0.,0.,1.));
#11128=DIRECTION('center_axis',(0.,0.,-1.));
#11129=DIRECTION('ref_axis',(1.,0.,0.));
#11130=DIRECTION('center_axis',(0.,0.,1.));
#11131=DIRECTION('ref_axis',(1.,0.,0.));
#11132=DIRECTION('center_axis',(0.,0.,1.));
#11133=DIRECTION('ref_axis',(1.,0.,0.));
#11134=DIRECTION('',(0.,0.,1.));
#11135=DIRECTION('center_axis',(0.,0.,-1.));
#11136=DIRECTION('ref_axis',(1.,0.,0.));
#11137=DIRECTION('center_axis',(0.,0.,1.));
#11138=DIRECTION('ref_axis',(1.,0.,0.));
#11139=DIRECTION('center_axis',(0.,0.,1.));
#11140=DIRECTION('ref_axis',(1.,0.,0.));
#11141=DIRECTION('',(0.,0.,1.));
#11142=DIRECTION('center_axis',(0.,0.,-1.));
#11143=DIRECTION('ref_axis',(1.,0.,0.));
#11144=DIRECTION('center_axis',(0.,0.,1.));
#11145=DIRECTION('ref_axis',(1.,0.,0.));
#11146=DIRECTION('center_axis',(0.,0.,1.));
#11147=DIRECTION('ref_axis',(1.,0.,0.));
#11148=DIRECTION('',(0.,0.,1.));
#11149=DIRECTION('center_axis',(0.,0.,-1.));
#11150=DIRECTION('ref_axis',(1.,0.,0.));
#11151=DIRECTION('center_axis',(0.,0.,1.));
#11152=DIRECTION('ref_axis',(1.,0.,0.));
#11153=DIRECTION('center_axis',(0.,0.,1.));
#11154=DIRECTION('ref_axis',(1.,0.,0.));
#11155=DIRECTION('',(0.,0.,1.));
#11156=DIRECTION('center_axis',(0.,0.,-1.));
#11157=DIRECTION('ref_axis',(1.,0.,0.));
#11158=DIRECTION('center_axis',(0.,0.,1.));
#11159=DIRECTION('ref_axis',(1.,0.,0.));
#11160=DIRECTION('center_axis',(0.,0.,1.));
#11161=DIRECTION('ref_axis',(1.,0.,0.));
#11162=DIRECTION('',(0.,0.,-1.));
#11163=DIRECTION('center_axis',(0.,0.,1.));
#11164=DIRECTION('ref_axis',(1.,0.,0.));
#11165=DIRECTION('center_axis',(0.,0.,1.));
#11166=DIRECTION('ref_axis',(1.,0.,0.));
#11167=DIRECTION('center_axis',(0.,0.,1.));
#11168=DIRECTION('ref_axis',(1.,0.,0.));
#11169=DIRECTION('axis',(0.,0.,1.));
#11170=DIRECTION('refdir',(1.,0.,0.));
#11171=DIRECTION('center_axis',(0.,1.,0.));
#11172=DIRECTION('ref_axis',(1.,0.,0.));
#11173=DIRECTION('',(0.,0.,1.));
#11174=DIRECTION('center_axis',(0.,1.,0.));
#11175=DIRECTION('ref_axis',(1.,0.,0.));
#11176=DIRECTION('center_axis',(0.,1.,0.));
#11177=DIRECTION('ref_axis',(1.,0.,0.));
#11178=DIRECTION('center_axis',(0.,1.,0.));
#11179=DIRECTION('ref_axis',(1.,0.,0.));
#11180=DIRECTION('center_axis',(0.,1.,0.));
#11181=DIRECTION('ref_axis',(1.,0.,0.));
#11182=DIRECTION('',(0.,1.,0.));
#11183=DIRECTION('center_axis',(0.,1.,0.));
#11184=DIRECTION('ref_axis',(1.,0.,0.));
#11185=DIRECTION('',(0.,0.,-1.));
#11186=DIRECTION('center_axis',(0.,0.,1.));
#11187=DIRECTION('ref_axis',(1.,0.,0.));
#11188=DIRECTION('center_axis',(0.,0.,-1.));
#11189=DIRECTION('ref_axis',(1.,0.,0.));
#11190=DIRECTION('',(0.,0.,-1.));
#11191=DIRECTION('center_axis',(0.,0.,-1.));
#11192=DIRECTION('ref_axis',(1.,0.,0.));
#11193=DIRECTION('center_axis',(0.,0.,1.));
#11194=DIRECTION('ref_axis',(1.,0.,0.));
#11195=DIRECTION('center_axis',(0.,0.,1.));
#11196=DIRECTION('ref_axis',(1.,0.,0.));
#11197=DIRECTION('',(0.,0.,-1.));
#11198=DIRECTION('center_axis',(0.,0.,1.));
#11199=DIRECTION('ref_axis',(1.,0.,0.));
#11200=DIRECTION('center_axis',(0.,0.,1.));
#11201=DIRECTION('ref_axis',(1.,0.,0.));
#11202=DIRECTION('center_axis',(0.,0.,1.));
#11203=DIRECTION('ref_axis',(1.,0.,0.));
#11204=DIRECTION('axis',(0.,0.,1.));
#11205=DIRECTION('refdir',(1.,0.,0.));
#11206=DIRECTION('center_axis',(0.,1.,0.));
#11207=DIRECTION('ref_axis',(0.,0.,1.));
#11208=DIRECTION('center_axis',(0.,-1.,0.));
#11209=DIRECTION('ref_axis',(1.,0.,0.));
#11210=DIRECTION('center_axis',(0.,-1.,0.));
#11211=DIRECTION('ref_axis',(1.,0.,0.));
#11212=DIRECTION('center_axis',(0.,-1.,0.));
#11213=DIRECTION('ref_axis',(1.,0.,0.));
#11214=DIRECTION('',(0.707106781186547,0.707106781186548,8.65956056235493E-17));
#11215=DIRECTION('center_axis',(0.,-1.,0.));
#11216=DIRECTION('ref_axis',(1.,0.,0.));
#11217=DIRECTION('center_axis',(0.,-1.,0.));
#11218=DIRECTION('ref_axis',(1.,0.,0.));
#11219=DIRECTION('',(0.,1.,0.));
#11220=DIRECTION('center_axis',(0.,1.,0.));
#11221=DIRECTION('ref_axis',(1.,0.,0.));
#11222=DIRECTION('center_axis',(0.,-1.,0.));
#11223=DIRECTION('ref_axis',(1.,0.,0.));
#11224=DIRECTION('',(-0.707106781186547,0.707106781186548,-8.65956056235493E-17));
#11225=DIRECTION('center_axis',(0.,-1.,0.));
#11226=DIRECTION('ref_axis',(0.,0.,-1.));
#11227=DIRECTION('center_axis',(0.,-1.,0.));
#11228=DIRECTION('ref_axis',(1.,0.,0.));
#11229=DIRECTION('center_axis',(0.,1.,0.));
#11230=DIRECTION('ref_axis',(1.,0.,0.));
#11231=DIRECTION('center_axis',(0.,1.,0.));
#11232=DIRECTION('ref_axis',(1.,0.,0.));
#11233=DIRECTION('',(-0.447213595499958,0.894427190999916,-5.47678698264203E-17));
#11234=DIRECTION('center_axis',(0.,-1.,0.));
#11235=DIRECTION('ref_axis',(1.,0.,0.));
#11236=DIRECTION('center_axis',(0.,1.,0.));
#11237=DIRECTION('ref_axis',(1.,0.,0.));
#11238=DIRECTION('',(0.,1.,0.));
#11239=DIRECTION('center_axis',(0.,1.,0.));
#11240=DIRECTION('ref_axis',(1.,0.,0.));
#11241=DIRECTION('center_axis',(0.,-1.,0.));
#11242=DIRECTION('ref_axis',(1.,0.,0.));
#11243=DIRECTION('',(-0.707106781186547,0.707106781186548,-8.65956056235493E-17));
#11244=DIRECTION('center_axis',(0.,-1.,0.));
#11245=DIRECTION('ref_axis',(0.,0.,-1.));
#11246=DIRECTION('center_axis',(0.866025403784439,0.,-0.5));
#11247=DIRECTION('ref_axis',(0.5,0.,0.866025403784439));
#11248=DIRECTION('',(-0.5,0.,-0.866025403784439));
#11249=DIRECTION('',(0.,-1.,0.));
#11250=DIRECTION('',(0.5,0.,0.866025403784439));
#11251=DIRECTION('',(0.,-1.,0.));
#11252=DIRECTION('center_axis',(1.60246890531964E-16,0.,-1.));
#11253=DIRECTION('ref_axis',(1.,0.,1.60246890531964E-16));
#11254=DIRECTION('',(-1.,0.,-1.60246890531964E-16));
#11255=DIRECTION('',(0.,-1.,0.));
#11256=DIRECTION('',(1.,0.,1.60246890531964E-16));
#11257=DIRECTION('center_axis',(-0.866025403784439,0.,-0.5));
#11258=DIRECTION('ref_axis',(0.5,0.,-0.866025403784439));
#11259=DIRECTION('',(-0.5,0.,0.866025403784439));
#11260=DIRECTION('',(0.,-1.,0.));
#11261=DIRECTION('',(0.5,0.,-0.866025403784439));
#11262=DIRECTION('center_axis',(-0.866025403784439,0.,0.5));
#11263=DIRECTION('ref_axis',(-0.5,0.,-0.866025403784439));
#11264=DIRECTION('',(0.5,0.,0.866025403784439));
#11265=DIRECTION('',(0.,-1.,0.));
#11266=DIRECTION('',(-0.5,0.,-0.866025403784439));
#11267=DIRECTION('center_axis',(-1.60246890531964E-16,0.,1.));
#11268=DIRECTION('ref_axis',(-1.,0.,-1.60246890531964E-16));
#11269=DIRECTION('',(1.,0.,1.60246890531964E-16));
#11270=DIRECTION('',(0.,-1.,0.));
#11271=DIRECTION('',(-1.,0.,-1.60246890531964E-16));
#11272=DIRECTION('center_axis',(0.866025403784439,0.,0.5));
#11273=DIRECTION('ref_axis',(-0.5,0.,0.866025403784439));
#11274=DIRECTION('',(0.5,0.,-0.866025403784439));
#11275=DIRECTION('',(-0.5,0.,0.866025403784439));
#11276=DIRECTION('center_axis',(0.,1.,0.));
#11277=DIRECTION('ref_axis',(1.,0.,0.));
#11278=DIRECTION('center_axis',(0.,-1.,0.));
#11279=DIRECTION('ref_axis',(0.,0.,-1.));
#11280=DIRECTION('',(0.,0.,1.));
#11281=DIRECTION('',(1.,0.,0.));
#11282=DIRECTION('',(0.,0.,1.));
#11283=DIRECTION('',(1.,0.,0.));
#11284=DIRECTION('',(0.,0.,1.));
#11285=DIRECTION('',(1.,0.,0.));
#11286=DIRECTION('',(0.,-1.,2.22044604925031E-16));
#11287=DIRECTION('',(1.,0.,0.));
#11288=DIRECTION('',(0.,-1.,2.22044604925031E-16));
#11289=DIRECTION('',(1.,0.,0.));
#11290=DIRECTION('',(0.,-1.,2.22044604925031E-16));
#11291=DIRECTION('',(1.,0.,0.));
#11292=DIRECTION('',(0.,-1.,2.22044604925031E-16));
#11293=DIRECTION('',(1.,0.,0.));
#11294=DIRECTION('',(0.,-1.,2.22044604925031E-16));
#11295=DIRECTION('',(1.,0.,0.));
#11296=DIRECTION('',(0.,-1.,2.22044604925031E-16));
#11297=DIRECTION('',(1.,0.,0.));
#11298=DIRECTION('',(0.,-1.,2.22044604925031E-16));
#11299=DIRECTION('',(1.,0.,0.));
#11300=DIRECTION('',(0.,-1.,2.22044604925031E-16));
#11301=DIRECTION('',(1.,0.,0.));
#11302=DIRECTION('',(0.,-1.,2.22044604925031E-16));
#11303=DIRECTION('',(1.,0.,0.));
#11304=DIRECTION('',(0.,0.,1.));
#11305=DIRECTION('',(1.,0.,0.));
#11306=DIRECTION('',(0.,0.,1.));
#11307=DIRECTION('',(1.,0.,0.));
#11308=DIRECTION('axis',(0.,0.,1.));
#11309=DIRECTION('refdir',(1.,0.,0.));
#11310=DIRECTION('center_axis',(0.866025403784439,0.,-0.5));
#11311=DIRECTION('ref_axis',(0.5,0.,0.866025403784439));
#11312=DIRECTION('',(0.5,0.,0.866025403784439));
#11313=DIRECTION('',(0.,-1.,0.));
#11314=DIRECTION('',(0.5,0.,0.866025403784439));
#11315=DIRECTION('',(0.,-1.,0.));
#11316=DIRECTION('center_axis',(1.92296268638356E-16,0.,-1.));
#11317=DIRECTION('ref_axis',(1.,0.,1.92296268638356E-16));
#11318=DIRECTION('',(1.,0.,1.92296268638356E-16));
#11319=DIRECTION('',(0.,-1.,0.));
#11320=DIRECTION('',(1.,0.,1.92296268638356E-16));
#11321=DIRECTION('center_axis',(-0.866025403784439,0.,-0.5));
#11322=DIRECTION('ref_axis',(0.5,0.,-0.866025403784439));
#11323=DIRECTION('',(0.5,0.,-0.866025403784439));
#11324=DIRECTION('',(0.,-1.,0.));
#11325=DIRECTION('',(0.5,0.,-0.866025403784438));
#11326=DIRECTION('center_axis',(-0.866025403784439,0.,0.5));
#11327=DIRECTION('ref_axis',(-0.5,0.,-0.866025403784439));
#11328=DIRECTION('',(-0.5,0.,-0.866025403784439));
#11329=DIRECTION('',(0.,-1.,0.));
#11330=DIRECTION('',(-0.5,0.,-0.866025403784439));
#11331=DIRECTION('center_axis',(-1.92296268638356E-16,0.,1.));
#11332=DIRECTION('ref_axis',(-1.,0.,-1.92296268638356E-16));
#11333=DIRECTION('',(-1.,0.,-1.92296268638356E-16));
#11334=DIRECTION('',(0.,-1.,0.));
#11335=DIRECTION('',(-1.,0.,-1.92296268638356E-16));
#11336=DIRECTION('center_axis',(0.866025403784439,0.,0.5));
#11337=DIRECTION('ref_axis',(-0.5,0.,0.866025403784439));
#11338=DIRECTION('',(-0.5,0.,0.866025403784439));
#11339=DIRECTION('',(-0.5,0.,0.866025403784439));
#11340=DIRECTION('center_axis',(0.,-1.,0.));
#11341=DIRECTION('ref_axis',(0.,0.,-1.));
#11342=DIRECTION('center_axis',(0.,1.,0.));
#11343=DIRECTION('ref_axis',(0.,0.,1.));
#11344=DIRECTION('center_axis',(0.,-1.,0.));
#11345=DIRECTION('ref_axis',(1.,0.,0.));
#11346=DIRECTION('center_axis',(0.,-1.,0.));
#11347=DIRECTION('ref_axis',(1.,0.,0.));
#11348=DIRECTION('center_axis',(0.,-1.,0.));
#11349=DIRECTION('ref_axis',(1.,0.,0.));
#11350=DIRECTION('',(0.707106781186547,0.707106781186548,8.65956056235493E-17));
#11351=DIRECTION('center_axis',(0.,-1.,0.));
#11352=DIRECTION('ref_axis',(1.,0.,0.));
#11353=DIRECTION('center_axis',(0.,1.,0.));
#11354=DIRECTION('ref_axis',(1.,0.,0.));
#11355=DIRECTION('',(0.,1.,0.));
#11356=DIRECTION('center_axis',(0.,1.,0.));
#11357=DIRECTION('ref_axis',(1.,0.,0.));
#11358=DIRECTION('center_axis',(0.,-1.,0.));
#11359=DIRECTION('ref_axis',(1.,0.,0.));
#11360=DIRECTION('',(-0.707106781186547,0.707106781186548,-8.65956056235493E-17));
#11361=DIRECTION('center_axis',(0.,-1.,0.));
#11362=DIRECTION('ref_axis',(0.,0.,-1.));
#11363=DIRECTION('',(0.,0.,1.));
#11364=DIRECTION('',(1.,0.,0.));
#11365=DIRECTION('',(0.,0.,1.));
#11366=DIRECTION('',(1.,0.,0.));
#11367=DIRECTION('',(0.,0.,1.));
#11368=DIRECTION('',(1.,0.,0.));
#11369=DIRECTION('',(0.,-1.,2.22044604925031E-16));
#11370=DIRECTION('',(1.,0.,0.));
#11371=DIRECTION('',(0.,-1.,2.22044604925031E-16));
#11372=DIRECTION('',(1.,0.,0.));
#11373=DIRECTION('',(0.,-1.,2.22044604925031E-16));
#11374=DIRECTION('',(1.,0.,0.));
#11375=DIRECTION('',(0.,0.,1.));
#11376=DIRECTION('',(1.,0.,0.));
#11377=DIRECTION('axis',(0.,0.,1.));
#11378=DIRECTION('refdir',(1.,0.,0.));
#11379=DIRECTION('axis',(0.,0.,1.));
#11380=DIRECTION('refdir',(1.,0.,0.));
#11381=DIRECTION('center_axis',(0.,0.,1.));
#11382=DIRECTION('ref_axis',(1.,0.,0.));
#11383=DIRECTION('center_axis',(0.,0.,1.));
#11384=DIRECTION('ref_axis',(1.,0.,0.));
#11385=DIRECTION('',(0.,0.,1.));
#11386=DIRECTION('center_axis',(0.,0.,-1.));
#11387=DIRECTION('ref_axis',(1.,0.,0.));
#11388=DIRECTION('center_axis',(0.,0.,1.));
#11389=DIRECTION('ref_axis',(1.,0.,0.));
#11390=DIRECTION('center_axis',(0.,0.,1.));
#11391=DIRECTION('ref_axis',(1.,0.,0.));
#11392=DIRECTION('',(0.,0.,1.));
#11393=DIRECTION('center_axis',(0.,0.,-1.));
#11394=DIRECTION('ref_axis',(1.,0.,0.));
#11395=DIRECTION('center_axis',(0.,0.,1.));
#11396=DIRECTION('ref_axis',(1.,0.,0.));
#11397=DIRECTION('center_axis',(0.,0.,1.));
#11398=DIRECTION('ref_axis',(1.,0.,0.));
#11399=DIRECTION('',(0.,0.,1.));
#11400=DIRECTION('center_axis',(0.,0.,-1.));
#11401=DIRECTION('ref_axis',(1.,0.,0.));
#11402=DIRECTION('center_axis',(0.,0.,1.));
#11403=DIRECTION('ref_axis',(1.,0.,0.));
#11404=DIRECTION('center_axis',(0.,0.,1.));
#11405=DIRECTION('ref_axis',(1.,0.,0.));
#11406=DIRECTION('',(0.,0.,1.));
#11407=DIRECTION('center_axis',(0.,0.,-1.));
#11408=DIRECTION('ref_axis',(1.,0.,0.));
#11409=DIRECTION('center_axis',(0.,1.,0.));
#11410=DIRECTION('ref_axis',(1.,0.,0.));
#11411=DIRECTION('center_axis',(0.,1.,0.));
#11412=DIRECTION('ref_axis',(1.,0.,0.));
#11413=DIRECTION('',(0.,1.,0.));
#11414=DIRECTION('center_axis',(0.,-1.,0.));
#11415=DIRECTION('ref_axis',(1.,0.,0.));
#11416=DIRECTION('center_axis',(0.,1.,0.));
#11417=DIRECTION('ref_axis',(1.,0.,0.));
#11418=DIRECTION('center_axis',(0.,1.,0.));
#11419=DIRECTION('ref_axis',(1.,0.,0.));
#11420=DIRECTION('',(0.,1.,0.));
#11421=DIRECTION('center_axis',(0.,-1.,0.));
#11422=DIRECTION('ref_axis',(1.,0.,0.));
#11423=DIRECTION('center_axis',(-1.,0.,0.));
#11424=DIRECTION('ref_axis',(0.,0.,1.));
#11425=DIRECTION('',(0.,0.,-1.));
#11426=DIRECTION('',(0.,1.,0.));
#11427=DIRECTION('',(0.,0.,1.));
#11428=DIRECTION('',(0.,1.,0.));
#11429=DIRECTION('center_axis',(1.,0.,0.));
#11430=DIRECTION('ref_axis',(0.,0.,-1.));
#11431=DIRECTION('',(0.,0.,1.));
#11432=DIRECTION('',(0.,-1.,0.));
#11433=DIRECTION('',(0.,0.,-1.));
#11434=DIRECTION('',(0.,1.,0.));
#11435=DIRECTION('center_axis',(0.,0.,1.));
#11436=DIRECTION('ref_axis',(1.,0.,0.));
#11437=DIRECTION('',(-1.,0.,0.));
#11438=DIRECTION('',(1.,0.,0.));
#11439=DIRECTION('center_axis',(0.,1.,0.));
#11440=DIRECTION('ref_axis',(0.,0.,1.));
#11441=DIRECTION('',(1.,0.,0.));
#11442=DIRECTION('center_axis',(0.,1.,0.));
#11443=DIRECTION('ref_axis',(1.,0.,0.));
#11444=DIRECTION('',(-1.,0.,0.));
#11445=DIRECTION('center_axis',(-1.,0.,0.));
#11446=DIRECTION('ref_axis',(0.,0.,1.));
#11447=DIRECTION('',(0.,0.,-1.));
#11448=DIRECTION('',(0.,1.,0.));
#11449=DIRECTION('',(0.,0.,1.));
#11450=DIRECTION('',(0.,1.,0.));
#11451=DIRECTION('center_axis',(1.,0.,0.));
#11452=DIRECTION('ref_axis',(0.,0.,-1.));
#11453=DIRECTION('',(0.,0.,1.));
#11454=DIRECTION('',(0.,-1.,0.));
#11455=DIRECTION('',(0.,0.,-1.));
#11456=DIRECTION('',(0.,1.,0.));
#11457=DIRECTION('center_axis',(0.,0.,1.));
#11458=DIRECTION('ref_axis',(1.,0.,0.));
#11459=DIRECTION('',(-1.,0.,0.));
#11460=DIRECTION('',(1.,0.,0.));
#11461=DIRECTION('center_axis',(0.,1.,0.));
#11462=DIRECTION('ref_axis',(0.,0.,1.));
#11463=DIRECTION('',(1.,0.,0.));
#11464=DIRECTION('center_axis',(0.,1.,0.));
#11465=DIRECTION('ref_axis',(1.,0.,0.));
#11466=DIRECTION('',(-1.,0.,0.));
#11467=DIRECTION('center_axis',(0.,1.,0.));
#11468=DIRECTION('ref_axis',(-1.,0.,0.));
#11469=DIRECTION('',(-1.,0.,0.));
#11470=DIRECTION('',(0.,0.,1.));
#11471=DIRECTION('',(-1.,0.,0.));
#11472=DIRECTION('',(0.,0.,1.));
#11473=DIRECTION('center_axis',(1.,0.,0.));
#11474=DIRECTION('ref_axis',(0.,1.,0.));
#11475=DIRECTION('',(0.,1.,0.));
#11476=DIRECTION('',(0.,1.,0.));
#11477=DIRECTION('',(0.,0.,1.));
#11478=DIRECTION('center_axis',(0.,-1.,0.));
#11479=DIRECTION('ref_axis',(1.,0.,0.));
#11480=DIRECTION('',(1.,0.,0.));
#11481=DIRECTION('',(1.,0.,0.));
#11482=DIRECTION('',(0.,0.,1.));
#11483=DIRECTION('center_axis',(-1.,0.,0.));
#11484=DIRECTION('ref_axis',(0.,-1.,0.));
#11485=DIRECTION('',(0.,-1.,0.));
#11486=DIRECTION('',(0.,-1.,0.));
#11487=DIRECTION('center_axis',(0.,0.,1.));
#11488=DIRECTION('ref_axis',(1.,0.,0.));
#11489=DIRECTION('center_axis',(0.,0.,1.));
#11490=DIRECTION('ref_axis',(1.,0.,0.));
#11491=DIRECTION('axis',(0.,0.,1.));
#11492=DIRECTION('refdir',(1.,0.,0.));
#11493=DIRECTION('center_axis',(0.,1.,0.));
#11494=DIRECTION('ref_axis',(1.,0.,0.));
#11495=DIRECTION('center_axis',(0.,1.,0.));
#11496=DIRECTION('ref_axis',(1.,0.,0.));
#11497=DIRECTION('',(0.,1.,0.));
#11498=DIRECTION('center_axis',(0.,-1.,0.));
#11499=DIRECTION('ref_axis',(1.,0.,0.));
#11500=DIRECTION('center_axis',(0.,1.,0.));
#11501=DIRECTION('ref_axis',(1.,0.,0.));
#11502=DIRECTION('center_axis',(0.,1.,0.));
#11503=DIRECTION('ref_axis',(1.,0.,0.));
#11504=DIRECTION('center_axis',(0.,1.,0.));
#11505=DIRECTION('ref_axis',(1.,0.,0.));
#11506=DIRECTION('center_axis',(0.,1.,0.));
#11507=DIRECTION('ref_axis',(1.,0.,0.));
#11508=DIRECTION('center_axis',(0.,1.,0.));
#11509=DIRECTION('ref_axis',(1.,0.,0.));
#11510=DIRECTION('',(0.,-1.,0.));
#11511=DIRECTION('center_axis',(0.,1.,0.));
#11512=DIRECTION('ref_axis',(1.,0.,0.));
#11513=DIRECTION('center_axis',(0.,1.,0.));
#11514=DIRECTION('ref_axis',(1.,0.,0.));
#11515=DIRECTION('center_axis',(0.,1.,0.));
#11516=DIRECTION('ref_axis',(1.,0.,0.));
#11517=DIRECTION('center_axis',(0.,1.,0.));
#11518=DIRECTION('ref_axis',(1.,0.,0.));
#11519=DIRECTION('',(0.,-1.,0.));
#11520=DIRECTION('center_axis',(0.,1.,0.));
#11521=DIRECTION('ref_axis',(1.,0.,0.));
#11522=DIRECTION('axis',(0.,0.,1.));
#11523=DIRECTION('refdir',(1.,0.,0.));
#11524=DIRECTION('center_axis',(0.,1.,0.));
#11525=DIRECTION('ref_axis',(1.,0.,0.));
#11526=DIRECTION('center_axis',(0.,-1.,0.));
#11527=DIRECTION('ref_axis',(1.,0.,0.));
#11528=DIRECTION('',(0.,-1.,0.));
#11529=DIRECTION('center_axis',(0.,-1.,0.));
#11530=DIRECTION('ref_axis',(1.,0.,0.));
#11531=DIRECTION('center_axis',(0.,1.,0.));
#11532=DIRECTION('ref_axis',(1.,0.,0.));
#11533=DIRECTION('center_axis',(0.,1.,0.));
#11534=DIRECTION('ref_axis',(1.,0.,0.));
#11535=DIRECTION('',(0.,-1.,0.));
#11536=DIRECTION('center_axis',(0.,1.,0.));
#11537=DIRECTION('ref_axis',(1.,0.,0.));
#11538=DIRECTION('center_axis',(0.,1.,0.));
#11539=DIRECTION('ref_axis',(1.,0.,0.));
#11540=DIRECTION('center_axis',(0.,1.,0.));
#11541=DIRECTION('ref_axis',(1.,0.,0.));
#11542=DIRECTION('axis',(0.,0.,1.));
#11543=DIRECTION('refdir',(1.,0.,0.));
#11544=DIRECTION('center_axis',(0.,1.,0.));
#11545=DIRECTION('ref_axis',(1.,0.,0.));
#11546=DIRECTION('center_axis',(0.,-1.,0.));
#11547=DIRECTION('ref_axis',(1.,0.,0.));
#11548=DIRECTION('',(0.,-1.,0.));
#11549=DIRECTION('center_axis',(0.,-1.,0.));
#11550=DIRECTION('ref_axis',(1.,0.,0.));
#11551=DIRECTION('center_axis',(0.,1.,0.));
#11552=DIRECTION('ref_axis',(1.,0.,0.));
#11553=DIRECTION('center_axis',(0.,1.,0.));
#11554=DIRECTION('ref_axis',(1.,0.,0.));
#11555=DIRECTION('',(0.,-1.,0.));
#11556=DIRECTION('center_axis',(0.,1.,0.));
#11557=DIRECTION('ref_axis',(1.,0.,0.));
#11558=DIRECTION('center_axis',(0.,1.,0.));
#11559=DIRECTION('ref_axis',(1.,0.,0.));
#11560=DIRECTION('center_axis',(0.,1.,0.));
#11561=DIRECTION('ref_axis',(1.,0.,0.));
#11562=DIRECTION('axis',(0.,0.,1.));
#11563=DIRECTION('refdir',(1.,0.,0.));
#11564=DIRECTION('center_axis',(0.,1.,0.));
#11565=DIRECTION('ref_axis',(1.,0.,0.));
#11566=DIRECTION('center_axis',(0.,-1.,0.));
#11567=DIRECTION('ref_axis',(1.,0.,0.));
#11568=DIRECTION('',(0.,-1.,0.));
#11569=DIRECTION('center_axis',(0.,-1.,0.));
#11570=DIRECTION('ref_axis',(1.,0.,0.));
#11571=DIRECTION('center_axis',(0.,1.,0.));
#11572=DIRECTION('ref_axis',(1.,0.,0.));
#11573=DIRECTION('center_axis',(0.,1.,0.));
#11574=DIRECTION('ref_axis',(1.,0.,0.));
#11575=DIRECTION('',(0.,-1.,0.));
#11576=DIRECTION('center_axis',(0.,1.,0.));
#11577=DIRECTION('ref_axis',(1.,0.,0.));
#11578=DIRECTION('center_axis',(0.,1.,0.));
#11579=DIRECTION('ref_axis',(1.,0.,0.));
#11580=DIRECTION('center_axis',(0.,1.,0.));
#11581=DIRECTION('ref_axis',(1.,0.,0.));
#11582=DIRECTION('axis',(0.,0.,1.));
#11583=DIRECTION('refdir',(1.,0.,0.));
#11584=DIRECTION('axis',(0.,0.,1.));
#11585=DIRECTION('refdir',(1.,0.,0.));
#11586=DIRECTION('center_axis',(0.,0.,1.));
#11587=DIRECTION('ref_axis',(1.,0.,0.));
#11588=DIRECTION('center_axis',(0.,0.,1.));
#11589=DIRECTION('ref_axis',(1.,0.,0.));
#11590=DIRECTION('',(0.,0.,1.));
#11591=DIRECTION('center_axis',(0.,0.,-1.));
#11592=DIRECTION('ref_axis',(1.,0.,0.));
#11593=DIRECTION('center_axis',(0.,0.,1.));
#11594=DIRECTION('ref_axis',(1.,0.,0.));
#11595=DIRECTION('center_axis',(0.,0.,1.));
#11596=DIRECTION('ref_axis',(1.,0.,0.));
#11597=DIRECTION('',(0.,0.,1.));
#11598=DIRECTION('center_axis',(0.,0.,-1.));
#11599=DIRECTION('ref_axis',(1.,0.,0.));
#11600=DIRECTION('center_axis',(0.,0.,1.));
#11601=DIRECTION('ref_axis',(1.,0.,0.));
#11602=DIRECTION('center_axis',(0.,0.,1.));
#11603=DIRECTION('ref_axis',(1.,0.,0.));
#11604=DIRECTION('',(0.,0.,1.));
#11605=DIRECTION('center_axis',(0.,0.,-1.));
#11606=DIRECTION('ref_axis',(1.,0.,0.));
#11607=DIRECTION('center_axis',(0.,0.,1.));
#11608=DIRECTION('ref_axis',(1.,0.,0.));
#11609=DIRECTION('center_axis',(0.,0.,1.));
#11610=DIRECTION('ref_axis',(1.,0.,0.));
#11611=DIRECTION('',(0.,0.,1.));
#11612=DIRECTION('center_axis',(0.,0.,-1.));
#11613=DIRECTION('ref_axis',(1.,0.,0.));
#11614=DIRECTION('center_axis',(0.,1.,0.));
#11615=DIRECTION('ref_axis',(1.,0.,0.));
#11616=DIRECTION('center_axis',(0.,1.,0.));
#11617=DIRECTION('ref_axis',(1.,0.,0.));
#11618=DIRECTION('',(0.,1.,0.));
#11619=DIRECTION('center_axis',(0.,-1.,0.));
#11620=DIRECTION('ref_axis',(1.,0.,0.));
#11621=DIRECTION('center_axis',(0.,1.,0.));
#11622=DIRECTION('ref_axis',(1.,0.,0.));
#11623=DIRECTION('center_axis',(0.,1.,0.));
#11624=DIRECTION('ref_axis',(1.,0.,0.));
#11625=DIRECTION('',(0.,1.,0.));
#11626=DIRECTION('center_axis',(0.,-1.,0.));
#11627=DIRECTION('ref_axis',(1.,0.,0.));
#11628=DIRECTION('center_axis',(-1.,0.,0.));
#11629=DIRECTION('ref_axis',(0.,0.,1.));
#11630=DIRECTION('',(0.,0.,-1.));
#11631=DIRECTION('',(0.,1.,0.));
#11632=DIRECTION('',(0.,0.,1.));
#11633=DIRECTION('',(0.,1.,0.));
#11634=DIRECTION('center_axis',(1.,0.,0.));
#11635=DIRECTION('ref_axis',(0.,0.,-1.));
#11636=DIRECTION('',(0.,0.,1.));
#11637=DIRECTION('',(0.,-1.,0.));
#11638=DIRECTION('',(0.,0.,-1.));
#11639=DIRECTION('',(0.,1.,0.));
#11640=DIRECTION('center_axis',(0.,0.,1.));
#11641=DIRECTION('ref_axis',(1.,0.,0.));
#11642=DIRECTION('',(-1.,0.,0.));
#11643=DIRECTION('',(1.,0.,0.));
#11644=DIRECTION('center_axis',(0.,1.,0.));
#11645=DIRECTION('ref_axis',(0.,0.,1.));
#11646=DIRECTION('',(1.,0.,0.));
#11647=DIRECTION('center_axis',(0.,1.,0.));
#11648=DIRECTION('ref_axis',(1.,0.,0.));
#11649=DIRECTION('',(-1.,0.,0.));
#11650=DIRECTION('center_axis',(-1.,0.,0.));
#11651=DIRECTION('ref_axis',(0.,0.,1.));
#11652=DIRECTION('',(0.,0.,-1.));
#11653=DIRECTION('',(0.,1.,0.));
#11654=DIRECTION('',(0.,0.,1.));
#11655=DIRECTION('',(0.,1.,0.));
#11656=DIRECTION('center_axis',(1.,0.,0.));
#11657=DIRECTION('ref_axis',(0.,0.,-1.));
#11658=DIRECTION('',(0.,0.,1.));
#11659=DIRECTION('',(0.,-1.,0.));
#11660=DIRECTION('',(0.,0.,-1.));
#11661=DIRECTION('',(0.,1.,0.));
#11662=DIRECTION('center_axis',(0.,0.,1.));
#11663=DIRECTION('ref_axis',(1.,0.,0.));
#11664=DIRECTION('',(-1.,0.,0.));
#11665=DIRECTION('',(1.,0.,0.));
#11666=DIRECTION('center_axis',(0.,1.,0.));
#11667=DIRECTION('ref_axis',(0.,0.,1.));
#11668=DIRECTION('',(1.,0.,0.));
#11669=DIRECTION('center_axis',(0.,1.,0.));
#11670=DIRECTION('ref_axis',(1.,0.,0.));
#11671=DIRECTION('',(-1.,0.,0.));
#11672=DIRECTION('center_axis',(0.,1.,0.));
#11673=DIRECTION('ref_axis',(-1.,0.,0.));
#11674=DIRECTION('',(-1.,0.,0.));
#11675=DIRECTION('',(0.,0.,1.));
#11676=DIRECTION('',(-1.,0.,0.));
#11677=DIRECTION('',(0.,0.,1.));
#11678=DIRECTION('center_axis',(1.,0.,0.));
#11679=DIRECTION('ref_axis',(0.,1.,0.));
#11680=DIRECTION('',(0.,1.,0.));
#11681=DIRECTION('',(0.,1.,0.));
#11682=DIRECTION('',(0.,0.,1.));
#11683=DIRECTION('center_axis',(0.,-1.,0.));
#11684=DIRECTION('ref_axis',(1.,0.,0.));
#11685=DIRECTION('',(1.,0.,0.));
#11686=DIRECTION('',(1.,0.,0.));
#11687=DIRECTION('',(0.,0.,1.));
#11688=DIRECTION('center_axis',(-1.,0.,0.));
#11689=DIRECTION('ref_axis',(0.,-1.,0.));
#11690=DIRECTION('',(0.,-1.,0.));
#11691=DIRECTION('',(0.,-1.,0.));
#11692=DIRECTION('center_axis',(0.,0.,1.));
#11693=DIRECTION('ref_axis',(1.,0.,0.));
#11694=DIRECTION('center_axis',(0.,0.,1.));
#11695=DIRECTION('ref_axis',(1.,0.,0.));
#11696=DIRECTION('axis',(0.,0.,1.));
#11697=DIRECTION('refdir',(1.,0.,0.));
#11698=DIRECTION('center_axis',(0.,1.,0.));
#11699=DIRECTION('ref_axis',(1.,0.,0.));
#11700=DIRECTION('center_axis',(0.,1.,0.));
#11701=DIRECTION('ref_axis',(1.,0.,0.));
#11702=DIRECTION('',(0.,1.,0.));
#11703=DIRECTION('center_axis',(0.,-1.,0.));
#11704=DIRECTION('ref_axis',(1.,0.,0.));
#11705=DIRECTION('center_axis',(0.,1.,0.));
#11706=DIRECTION('ref_axis',(1.,0.,0.));
#11707=DIRECTION('center_axis',(0.,1.,0.));
#11708=DIRECTION('ref_axis',(1.,0.,0.));
#11709=DIRECTION('center_axis',(0.,1.,0.));
#11710=DIRECTION('ref_axis',(1.,0.,0.));
#11711=DIRECTION('center_axis',(0.,1.,0.));
#11712=DIRECTION('ref_axis',(1.,0.,0.));
#11713=DIRECTION('center_axis',(0.,1.,0.));
#11714=DIRECTION('ref_axis',(1.,0.,0.));
#11715=DIRECTION('',(0.,-1.,0.));
#11716=DIRECTION('center_axis',(0.,1.,0.));
#11717=DIRECTION('ref_axis',(1.,0.,0.));
#11718=DIRECTION('center_axis',(0.,1.,0.));
#11719=DIRECTION('ref_axis',(1.,0.,0.));
#11720=DIRECTION('center_axis',(0.,1.,0.));
#11721=DIRECTION('ref_axis',(1.,0.,0.));
#11722=DIRECTION('center_axis',(0.,1.,0.));
#11723=DIRECTION('ref_axis',(1.,0.,0.));
#11724=DIRECTION('',(0.,-1.,0.));
#11725=DIRECTION('center_axis',(0.,1.,0.));
#11726=DIRECTION('ref_axis',(1.,0.,0.));
#11727=DIRECTION('axis',(0.,0.,1.));
#11728=DIRECTION('refdir',(1.,0.,0.));
#11729=DIRECTION('center_axis',(0.,1.,0.));
#11730=DIRECTION('ref_axis',(1.,0.,0.));
#11731=DIRECTION('center_axis',(0.,-1.,0.));
#11732=DIRECTION('ref_axis',(1.,0.,0.));
#11733=DIRECTION('',(0.,-1.,0.));
#11734=DIRECTION('center_axis',(0.,-1.,0.));
#11735=DIRECTION('ref_axis',(1.,0.,0.));
#11736=DIRECTION('center_axis',(0.,1.,0.));
#11737=DIRECTION('ref_axis',(1.,0.,0.));
#11738=DIRECTION('center_axis',(0.,1.,0.));
#11739=DIRECTION('ref_axis',(1.,0.,0.));
#11740=DIRECTION('',(0.,-1.,0.));
#11741=DIRECTION('center_axis',(0.,1.,0.));
#11742=DIRECTION('ref_axis',(1.,0.,0.));
#11743=DIRECTION('center_axis',(0.,1.,0.));
#11744=DIRECTION('ref_axis',(1.,0.,0.));
#11745=DIRECTION('center_axis',(0.,1.,0.));
#11746=DIRECTION('ref_axis',(1.,0.,0.));
#11747=DIRECTION('axis',(0.,0.,1.));
#11748=DIRECTION('refdir',(1.,0.,0.));
#11749=DIRECTION('center_axis',(0.,1.,0.));
#11750=DIRECTION('ref_axis',(1.,0.,0.));
#11751=DIRECTION('center_axis',(0.,-1.,0.));
#11752=DIRECTION('ref_axis',(1.,0.,0.));
#11753=DIRECTION('',(0.,-1.,0.));
#11754=DIRECTION('center_axis',(0.,-1.,0.));
#11755=DIRECTION('ref_axis',(1.,0.,0.));
#11756=DIRECTION('center_axis',(0.,1.,0.));
#11757=DIRECTION('ref_axis',(1.,0.,0.));
#11758=DIRECTION('center_axis',(0.,1.,0.));
#11759=DIRECTION('ref_axis',(1.,0.,0.));
#11760=DIRECTION('',(0.,-1.,0.));
#11761=DIRECTION('center_axis',(0.,1.,0.));
#11762=DIRECTION('ref_axis',(1.,0.,0.));
#11763=DIRECTION('center_axis',(0.,1.,0.));
#11764=DIRECTION('ref_axis',(1.,0.,0.));
#11765=DIRECTION('center_axis',(0.,1.,0.));
#11766=DIRECTION('ref_axis',(1.,0.,0.));
#11767=DIRECTION('axis',(0.,0.,1.));
#11768=DIRECTION('refdir',(1.,0.,0.));
#11769=DIRECTION('center_axis',(0.,1.,0.));
#11770=DIRECTION('ref_axis',(1.,0.,0.));
#11771=DIRECTION('center_axis',(0.,-1.,0.));
#11772=DIRECTION('ref_axis',(1.,0.,0.));
#11773=DIRECTION('',(0.,-1.,0.));
#11774=DIRECTION('center_axis',(0.,-1.,0.));
#11775=DIRECTION('ref_axis',(1.,0.,0.));
#11776=DIRECTION('center_axis',(0.,1.,0.));
#11777=DIRECTION('ref_axis',(1.,0.,0.));
#11778=DIRECTION('center_axis',(0.,1.,0.));
#11779=DIRECTION('ref_axis',(1.,0.,0.));
#11780=DIRECTION('',(0.,-1.,0.));
#11781=DIRECTION('center_axis',(0.,1.,0.));
#11782=DIRECTION('ref_axis',(1.,0.,0.));
#11783=DIRECTION('center_axis',(0.,1.,0.));
#11784=DIRECTION('ref_axis',(1.,0.,0.));
#11785=DIRECTION('center_axis',(0.,1.,0.));
#11786=DIRECTION('ref_axis',(1.,0.,0.));
#11787=DIRECTION('axis',(0.,0.,1.));
#11788=DIRECTION('refdir',(1.,0.,0.));
#11789=DIRECTION('axis',(0.,0.,1.));
#11790=DIRECTION('refdir',(1.,0.,0.));
#11791=DIRECTION('center_axis',(0.,0.,1.));
#11792=DIRECTION('ref_axis',(1.,0.,0.));
#11793=DIRECTION('center_axis',(0.,0.,1.));
#11794=DIRECTION('ref_axis',(1.,0.,0.));
#11795=DIRECTION('',(0.,0.,1.));
#11796=DIRECTION('center_axis',(0.,0.,-1.));
#11797=DIRECTION('ref_axis',(1.,0.,0.));
#11798=DIRECTION('center_axis',(0.,0.,1.));
#11799=DIRECTION('ref_axis',(1.,0.,0.));
#11800=DIRECTION('center_axis',(0.,0.,1.));
#11801=DIRECTION('ref_axis',(1.,0.,0.));
#11802=DIRECTION('',(0.,0.,1.));
#11803=DIRECTION('center_axis',(0.,0.,-1.));
#11804=DIRECTION('ref_axis',(1.,0.,0.));
#11805=DIRECTION('center_axis',(0.,0.,1.));
#11806=DIRECTION('ref_axis',(1.,0.,0.));
#11807=DIRECTION('center_axis',(0.,0.,1.));
#11808=DIRECTION('ref_axis',(1.,0.,0.));
#11809=DIRECTION('',(0.,0.,1.));
#11810=DIRECTION('center_axis',(0.,0.,-1.));
#11811=DIRECTION('ref_axis',(1.,0.,0.));
#11812=DIRECTION('center_axis',(0.,0.,1.));
#11813=DIRECTION('ref_axis',(1.,0.,0.));
#11814=DIRECTION('center_axis',(0.,0.,1.));
#11815=DIRECTION('ref_axis',(1.,0.,0.));
#11816=DIRECTION('',(0.,0.,1.));
#11817=DIRECTION('center_axis',(0.,0.,-1.));
#11818=DIRECTION('ref_axis',(1.,0.,0.));
#11819=DIRECTION('center_axis',(0.,1.,0.));
#11820=DIRECTION('ref_axis',(1.,0.,0.));
#11821=DIRECTION('center_axis',(0.,1.,0.));
#11822=DIRECTION('ref_axis',(1.,0.,0.));
#11823=DIRECTION('',(0.,1.,0.));
#11824=DIRECTION('center_axis',(0.,-1.,0.));
#11825=DIRECTION('ref_axis',(1.,0.,0.));
#11826=DIRECTION('center_axis',(0.,1.,0.));
#11827=DIRECTION('ref_axis',(1.,0.,0.));
#11828=DIRECTION('center_axis',(0.,1.,0.));
#11829=DIRECTION('ref_axis',(1.,0.,0.));
#11830=DIRECTION('',(0.,1.,0.));
#11831=DIRECTION('center_axis',(0.,-1.,0.));
#11832=DIRECTION('ref_axis',(1.,0.,0.));
#11833=DIRECTION('center_axis',(-1.,0.,0.));
#11834=DIRECTION('ref_axis',(0.,0.,1.));
#11835=DIRECTION('',(0.,0.,-1.));
#11836=DIRECTION('',(0.,1.,0.));
#11837=DIRECTION('',(0.,0.,1.));
#11838=DIRECTION('',(0.,1.,0.));
#11839=DIRECTION('center_axis',(1.,0.,0.));
#11840=DIRECTION('ref_axis',(0.,0.,-1.));
#11841=DIRECTION('',(0.,0.,1.));
#11842=DIRECTION('',(0.,-1.,0.));
#11843=DIRECTION('',(0.,0.,-1.));
#11844=DIRECTION('',(0.,1.,0.));
#11845=DIRECTION('center_axis',(0.,0.,1.));
#11846=DIRECTION('ref_axis',(1.,0.,0.));
#11847=DIRECTION('',(-1.,0.,0.));
#11848=DIRECTION('',(1.,0.,0.));
#11849=DIRECTION('center_axis',(0.,1.,0.));
#11850=DIRECTION('ref_axis',(0.,0.,1.));
#11851=DIRECTION('',(1.,0.,0.));
#11852=DIRECTION('center_axis',(0.,1.,0.));
#11853=DIRECTION('ref_axis',(1.,0.,0.));
#11854=DIRECTION('',(-1.,0.,0.));
#11855=DIRECTION('center_axis',(-1.,0.,0.));
#11856=DIRECTION('ref_axis',(0.,0.,1.));
#11857=DIRECTION('',(0.,0.,-1.));
#11858=DIRECTION('',(0.,1.,0.));
#11859=DIRECTION('',(0.,0.,1.));
#11860=DIRECTION('',(0.,1.,0.));
#11861=DIRECTION('center_axis',(1.,0.,0.));
#11862=DIRECTION('ref_axis',(0.,0.,-1.));
#11863=DIRECTION('',(0.,0.,1.));
#11864=DIRECTION('',(0.,-1.,0.));
#11865=DIRECTION('',(0.,0.,-1.));
#11866=DIRECTION('',(0.,1.,0.));
#11867=DIRECTION('center_axis',(0.,0.,1.));
#11868=DIRECTION('ref_axis',(1.,0.,0.));
#11869=DIRECTION('',(-1.,0.,0.));
#11870=DIRECTION('',(1.,0.,0.));
#11871=DIRECTION('center_axis',(0.,1.,0.));
#11872=DIRECTION('ref_axis',(0.,0.,1.));
#11873=DIRECTION('',(1.,0.,0.));
#11874=DIRECTION('center_axis',(0.,1.,0.));
#11875=DIRECTION('ref_axis',(1.,0.,0.));
#11876=DIRECTION('',(-1.,0.,0.));
#11877=DIRECTION('center_axis',(0.,1.,0.));
#11878=DIRECTION('ref_axis',(-1.,0.,0.));
#11879=DIRECTION('',(-1.,0.,0.));
#11880=DIRECTION('',(0.,0.,1.));
#11881=DIRECTION('',(-1.,0.,0.));
#11882=DIRECTION('',(0.,0.,1.));
#11883=DIRECTION('center_axis',(1.,0.,0.));
#11884=DIRECTION('ref_axis',(0.,1.,0.));
#11885=DIRECTION('',(0.,1.,0.));
#11886=DIRECTION('',(0.,1.,0.));
#11887=DIRECTION('',(0.,0.,1.));
#11888=DIRECTION('center_axis',(0.,-1.,0.));
#11889=DIRECTION('ref_axis',(1.,0.,0.));
#11890=DIRECTION('',(1.,0.,0.));
#11891=DIRECTION('',(1.,0.,0.));
#11892=DIRECTION('',(0.,0.,1.));
#11893=DIRECTION('center_axis',(-1.,0.,0.));
#11894=DIRECTION('ref_axis',(0.,-1.,0.));
#11895=DIRECTION('',(0.,-1.,0.));
#11896=DIRECTION('',(0.,-1.,0.));
#11897=DIRECTION('center_axis',(0.,0.,1.));
#11898=DIRECTION('ref_axis',(1.,0.,0.));
#11899=DIRECTION('center_axis',(0.,0.,1.));
#11900=DIRECTION('ref_axis',(1.,0.,0.));
#11901=DIRECTION('axis',(0.,0.,1.));
#11902=DIRECTION('refdir',(1.,0.,0.));
#11903=DIRECTION('center_axis',(0.,1.,0.));
#11904=DIRECTION('ref_axis',(1.,0.,0.));
#11905=DIRECTION('center_axis',(0.,1.,0.));
#11906=DIRECTION('ref_axis',(1.,0.,0.));
#11907=DIRECTION('',(0.,1.,0.));
#11908=DIRECTION('center_axis',(0.,-1.,0.));
#11909=DIRECTION('ref_axis',(1.,0.,0.));
#11910=DIRECTION('center_axis',(0.,1.,0.));
#11911=DIRECTION('ref_axis',(1.,0.,0.));
#11912=DIRECTION('center_axis',(0.,1.,0.));
#11913=DIRECTION('ref_axis',(1.,0.,0.));
#11914=DIRECTION('center_axis',(0.,1.,0.));
#11915=DIRECTION('ref_axis',(1.,0.,0.));
#11916=DIRECTION('center_axis',(0.,1.,0.));
#11917=DIRECTION('ref_axis',(1.,0.,0.));
#11918=DIRECTION('center_axis',(0.,1.,0.));
#11919=DIRECTION('ref_axis',(1.,0.,0.));
#11920=DIRECTION('',(0.,-1.,0.));
#11921=DIRECTION('center_axis',(0.,1.,0.));
#11922=DIRECTION('ref_axis',(1.,0.,0.));
#11923=DIRECTION('center_axis',(0.,1.,0.));
#11924=DIRECTION('ref_axis',(1.,0.,0.));
#11925=DIRECTION('center_axis',(0.,1.,0.));
#11926=DIRECTION('ref_axis',(1.,0.,0.));
#11927=DIRECTION('center_axis',(0.,1.,0.));
#11928=DIRECTION('ref_axis',(1.,0.,0.));
#11929=DIRECTION('',(0.,-1.,0.));
#11930=DIRECTION('center_axis',(0.,1.,0.));
#11931=DIRECTION('ref_axis',(1.,0.,0.));
#11932=DIRECTION('axis',(0.,0.,1.));
#11933=DIRECTION('refdir',(1.,0.,0.));
#11934=DIRECTION('center_axis',(0.,1.,0.));
#11935=DIRECTION('ref_axis',(1.,0.,0.));
#11936=DIRECTION('center_axis',(0.,-1.,0.));
#11937=DIRECTION('ref_axis',(1.,0.,0.));
#11938=DIRECTION('',(0.,-1.,0.));
#11939=DIRECTION('center_axis',(0.,-1.,0.));
#11940=DIRECTION('ref_axis',(1.,0.,0.));
#11941=DIRECTION('center_axis',(0.,1.,0.));
#11942=DIRECTION('ref_axis',(1.,0.,0.));
#11943=DIRECTION('center_axis',(0.,1.,0.));
#11944=DIRECTION('ref_axis',(1.,0.,0.));
#11945=DIRECTION('',(0.,-1.,0.));
#11946=DIRECTION('center_axis',(0.,1.,0.));
#11947=DIRECTION('ref_axis',(1.,0.,0.));
#11948=DIRECTION('center_axis',(0.,1.,0.));
#11949=DIRECTION('ref_axis',(1.,0.,0.));
#11950=DIRECTION('center_axis',(0.,1.,0.));
#11951=DIRECTION('ref_axis',(1.,0.,0.));
#11952=DIRECTION('axis',(0.,0.,1.));
#11953=DIRECTION('refdir',(1.,0.,0.));
#11954=DIRECTION('center_axis',(0.,1.,0.));
#11955=DIRECTION('ref_axis',(1.,0.,0.));
#11956=DIRECTION('center_axis',(0.,-1.,0.));
#11957=DIRECTION('ref_axis',(1.,0.,0.));
#11958=DIRECTION('',(0.,-1.,0.));
#11959=DIRECTION('center_axis',(0.,-1.,0.));
#11960=DIRECTION('ref_axis',(1.,0.,0.));
#11961=DIRECTION('center_axis',(0.,1.,0.));
#11962=DIRECTION('ref_axis',(1.,0.,0.));
#11963=DIRECTION('center_axis',(0.,1.,0.));
#11964=DIRECTION('ref_axis',(1.,0.,0.));
#11965=DIRECTION('',(0.,-1.,0.));
#11966=DIRECTION('center_axis',(0.,1.,0.));
#11967=DIRECTION('ref_axis',(1.,0.,0.));
#11968=DIRECTION('center_axis',(0.,1.,0.));
#11969=DIRECTION('ref_axis',(1.,0.,0.));
#11970=DIRECTION('center_axis',(0.,1.,0.));
#11971=DIRECTION('ref_axis',(1.,0.,0.));
#11972=DIRECTION('axis',(0.,0.,1.));
#11973=DIRECTION('refdir',(1.,0.,0.));
#11974=DIRECTION('center_axis',(0.,1.,0.));
#11975=DIRECTION('ref_axis',(1.,0.,0.));
#11976=DIRECTION('center_axis',(0.,-1.,0.));
#11977=DIRECTION('ref_axis',(1.,0.,0.));
#11978=DIRECTION('',(0.,-1.,0.));
#11979=DIRECTION('center_axis',(0.,-1.,0.));
#11980=DIRECTION('ref_axis',(1.,0.,0.));
#11981=DIRECTION('center_axis',(0.,1.,0.));
#11982=DIRECTION('ref_axis',(1.,0.,0.));
#11983=DIRECTION('center_axis',(0.,1.,0.));
#11984=DIRECTION('ref_axis',(1.,0.,0.));
#11985=DIRECTION('',(0.,-1.,0.));
#11986=DIRECTION('center_axis',(0.,1.,0.));
#11987=DIRECTION('ref_axis',(1.,0.,0.));
#11988=DIRECTION('center_axis',(0.,1.,0.));
#11989=DIRECTION('ref_axis',(1.,0.,0.));
#11990=DIRECTION('center_axis',(0.,1.,0.));
#11991=DIRECTION('ref_axis',(1.,0.,0.));
#11992=DIRECTION('axis',(0.,0.,1.));
#11993=DIRECTION('refdir',(1.,0.,0.));
#11994=DIRECTION('axis',(0.,0.,1.));
#11995=DIRECTION('refdir',(1.,0.,0.));
#11996=DIRECTION('center_axis',(0.,0.,1.));
#11997=DIRECTION('ref_axis',(1.,0.,0.));
#11998=DIRECTION('center_axis',(0.,0.,1.));
#11999=DIRECTION('ref_axis',(1.,0.,0.));
#12000=DIRECTION('',(0.,0.,1.));
#12001=DIRECTION('center_axis',(0.,0.,-1.));
#12002=DIRECTION('ref_axis',(1.,0.,0.));
#12003=DIRECTION('center_axis',(0.,0.,1.));
#12004=DIRECTION('ref_axis',(1.,0.,0.));
#12005=DIRECTION('center_axis',(0.,0.,1.));
#12006=DIRECTION('ref_axis',(1.,0.,0.));
#12007=DIRECTION('',(0.,0.,1.));
#12008=DIRECTION('center_axis',(0.,0.,-1.));
#12009=DIRECTION('ref_axis',(1.,0.,0.));
#12010=DIRECTION('center_axis',(0.,0.,1.));
#12011=DIRECTION('ref_axis',(1.,0.,0.));
#12012=DIRECTION('center_axis',(0.,0.,1.));
#12013=DIRECTION('ref_axis',(1.,0.,0.));
#12014=DIRECTION('',(0.,0.,1.));
#12015=DIRECTION('center_axis',(0.,0.,-1.));
#12016=DIRECTION('ref_axis',(1.,0.,0.));
#12017=DIRECTION('center_axis',(0.,0.,1.));
#12018=DIRECTION('ref_axis',(1.,0.,0.));
#12019=DIRECTION('center_axis',(0.,0.,1.));
#12020=DIRECTION('ref_axis',(1.,0.,0.));
#12021=DIRECTION('',(0.,0.,1.));
#12022=DIRECTION('center_axis',(0.,0.,-1.));
#12023=DIRECTION('ref_axis',(1.,0.,0.));
#12024=DIRECTION('center_axis',(0.,1.,0.));
#12025=DIRECTION('ref_axis',(1.,0.,0.));
#12026=DIRECTION('center_axis',(0.,1.,0.));
#12027=DIRECTION('ref_axis',(1.,0.,0.));
#12028=DIRECTION('',(0.,1.,0.));
#12029=DIRECTION('center_axis',(0.,-1.,0.));
#12030=DIRECTION('ref_axis',(1.,0.,0.));
#12031=DIRECTION('center_axis',(0.,1.,0.));
#12032=DIRECTION('ref_axis',(1.,0.,0.));
#12033=DIRECTION('center_axis',(0.,1.,0.));
#12034=DIRECTION('ref_axis',(1.,0.,0.));
#12035=DIRECTION('',(0.,1.,0.));
#12036=DIRECTION('center_axis',(0.,-1.,0.));
#12037=DIRECTION('ref_axis',(1.,0.,0.));
#12038=DIRECTION('center_axis',(-1.,0.,0.));
#12039=DIRECTION('ref_axis',(0.,0.,1.));
#12040=DIRECTION('',(0.,0.,-1.));
#12041=DIRECTION('',(0.,1.,0.));
#12042=DIRECTION('',(0.,0.,1.));
#12043=DIRECTION('',(0.,1.,0.));
#12044=DIRECTION('center_axis',(1.,0.,0.));
#12045=DIRECTION('ref_axis',(0.,0.,-1.));
#12046=DIRECTION('',(0.,0.,1.));
#12047=DIRECTION('',(0.,-1.,0.));
#12048=DIRECTION('',(0.,0.,-1.));
#12049=DIRECTION('',(0.,1.,0.));
#12050=DIRECTION('center_axis',(0.,0.,1.));
#12051=DIRECTION('ref_axis',(1.,0.,0.));
#12052=DIRECTION('',(-1.,0.,0.));
#12053=DIRECTION('',(1.,0.,0.));
#12054=DIRECTION('center_axis',(0.,1.,0.));
#12055=DIRECTION('ref_axis',(0.,0.,1.));
#12056=DIRECTION('',(1.,0.,0.));
#12057=DIRECTION('center_axis',(0.,1.,0.));
#12058=DIRECTION('ref_axis',(1.,0.,0.));
#12059=DIRECTION('',(-1.,0.,0.));
#12060=DIRECTION('center_axis',(-1.,0.,0.));
#12061=DIRECTION('ref_axis',(0.,0.,1.));
#12062=DIRECTION('',(0.,0.,-1.));
#12063=DIRECTION('',(0.,1.,0.));
#12064=DIRECTION('',(0.,0.,1.));
#12065=DIRECTION('',(0.,1.,0.));
#12066=DIRECTION('center_axis',(1.,0.,0.));
#12067=DIRECTION('ref_axis',(0.,0.,-1.));
#12068=DIRECTION('',(0.,0.,1.));
#12069=DIRECTION('',(0.,-1.,0.));
#12070=DIRECTION('',(0.,0.,-1.));
#12071=DIRECTION('',(0.,1.,0.));
#12072=DIRECTION('center_axis',(0.,0.,1.));
#12073=DIRECTION('ref_axis',(1.,0.,0.));
#12074=DIRECTION('',(-1.,0.,0.));
#12075=DIRECTION('',(1.,0.,0.));
#12076=DIRECTION('center_axis',(0.,1.,0.));
#12077=DIRECTION('ref_axis',(0.,0.,1.));
#12078=DIRECTION('',(1.,0.,0.));
#12079=DIRECTION('center_axis',(0.,1.,0.));
#12080=DIRECTION('ref_axis',(1.,0.,0.));
#12081=DIRECTION('',(-1.,0.,0.));
#12082=DIRECTION('center_axis',(0.,1.,0.));
#12083=DIRECTION('ref_axis',(-1.,0.,0.));
#12084=DIRECTION('',(-1.,0.,0.));
#12085=DIRECTION('',(0.,0.,1.));
#12086=DIRECTION('',(-1.,0.,0.));
#12087=DIRECTION('',(0.,0.,1.));
#12088=DIRECTION('center_axis',(1.,0.,0.));
#12089=DIRECTION('ref_axis',(0.,1.,0.));
#12090=DIRECTION('',(0.,1.,0.));
#12091=DIRECTION('',(0.,1.,0.));
#12092=DIRECTION('',(0.,0.,1.));
#12093=DIRECTION('center_axis',(0.,-1.,0.));
#12094=DIRECTION('ref_axis',(1.,0.,0.));
#12095=DIRECTION('',(1.,0.,0.));
#12096=DIRECTION('',(1.,0.,0.));
#12097=DIRECTION('',(0.,0.,1.));
#12098=DIRECTION('center_axis',(-1.,0.,0.));
#12099=DIRECTION('ref_axis',(0.,-1.,0.));
#12100=DIRECTION('',(0.,-1.,0.));
#12101=DIRECTION('',(0.,-1.,0.));
#12102=DIRECTION('center_axis',(0.,0.,1.));
#12103=DIRECTION('ref_axis',(1.,0.,0.));
#12104=DIRECTION('center_axis',(0.,0.,1.));
#12105=DIRECTION('ref_axis',(1.,0.,0.));
#12106=DIRECTION('axis',(0.,0.,1.));
#12107=DIRECTION('refdir',(1.,0.,0.));
#12108=DIRECTION('center_axis',(0.,1.,0.));
#12109=DIRECTION('ref_axis',(1.,0.,0.));
#12110=DIRECTION('center_axis',(0.,1.,0.));
#12111=DIRECTION('ref_axis',(1.,0.,0.));
#12112=DIRECTION('',(0.,1.,0.));
#12113=DIRECTION('center_axis',(0.,-1.,0.));
#12114=DIRECTION('ref_axis',(1.,0.,0.));
#12115=DIRECTION('center_axis',(0.,1.,0.));
#12116=DIRECTION('ref_axis',(1.,0.,0.));
#12117=DIRECTION('center_axis',(0.,1.,0.));
#12118=DIRECTION('ref_axis',(1.,0.,0.));
#12119=DIRECTION('center_axis',(0.,1.,0.));
#12120=DIRECTION('ref_axis',(1.,0.,0.));
#12121=DIRECTION('center_axis',(0.,1.,0.));
#12122=DIRECTION('ref_axis',(1.,0.,0.));
#12123=DIRECTION('center_axis',(0.,1.,0.));
#12124=DIRECTION('ref_axis',(1.,0.,0.));
#12125=DIRECTION('',(0.,-1.,0.));
#12126=DIRECTION('center_axis',(0.,1.,0.));
#12127=DIRECTION('ref_axis',(1.,0.,0.));
#12128=DIRECTION('center_axis',(0.,1.,0.));
#12129=DIRECTION('ref_axis',(1.,0.,0.));
#12130=DIRECTION('center_axis',(0.,1.,0.));
#12131=DIRECTION('ref_axis',(1.,0.,0.));
#12132=DIRECTION('center_axis',(0.,1.,0.));
#12133=DIRECTION('ref_axis',(1.,0.,0.));
#12134=DIRECTION('',(0.,-1.,0.));
#12135=DIRECTION('center_axis',(0.,1.,0.));
#12136=DIRECTION('ref_axis',(1.,0.,0.));
#12137=DIRECTION('axis',(0.,0.,1.));
#12138=DIRECTION('refdir',(1.,0.,0.));
#12139=DIRECTION('center_axis',(0.,1.,0.));
#12140=DIRECTION('ref_axis',(1.,0.,0.));
#12141=DIRECTION('center_axis',(0.,-1.,0.));
#12142=DIRECTION('ref_axis',(1.,0.,0.));
#12143=DIRECTION('',(0.,-1.,0.));
#12144=DIRECTION('center_axis',(0.,-1.,0.));
#12145=DIRECTION('ref_axis',(1.,0.,0.));
#12146=DIRECTION('center_axis',(0.,1.,0.));
#12147=DIRECTION('ref_axis',(1.,0.,0.));
#12148=DIRECTION('center_axis',(0.,1.,0.));
#12149=DIRECTION('ref_axis',(1.,0.,0.));
#12150=DIRECTION('',(0.,-1.,0.));
#12151=DIRECTION('center_axis',(0.,1.,0.));
#12152=DIRECTION('ref_axis',(1.,0.,0.));
#12153=DIRECTION('center_axis',(0.,1.,0.));
#12154=DIRECTION('ref_axis',(1.,0.,0.));
#12155=DIRECTION('center_axis',(0.,1.,0.));
#12156=DIRECTION('ref_axis',(1.,0.,0.));
#12157=DIRECTION('axis',(0.,0.,1.));
#12158=DIRECTION('refdir',(1.,0.,0.));
#12159=DIRECTION('center_axis',(0.,1.,0.));
#12160=DIRECTION('ref_axis',(1.,0.,0.));
#12161=DIRECTION('center_axis',(0.,-1.,0.));
#12162=DIRECTION('ref_axis',(1.,0.,0.));
#12163=DIRECTION('',(0.,-1.,0.));
#12164=DIRECTION('center_axis',(0.,-1.,0.));
#12165=DIRECTION('ref_axis',(1.,0.,0.));
#12166=DIRECTION('center_axis',(0.,1.,0.));
#12167=DIRECTION('ref_axis',(1.,0.,0.));
#12168=DIRECTION('center_axis',(0.,1.,0.));
#12169=DIRECTION('ref_axis',(1.,0.,0.));
#12170=DIRECTION('',(0.,-1.,0.));
#12171=DIRECTION('center_axis',(0.,1.,0.));
#12172=DIRECTION('ref_axis',(1.,0.,0.));
#12173=DIRECTION('center_axis',(0.,1.,0.));
#12174=DIRECTION('ref_axis',(1.,0.,0.));
#12175=DIRECTION('center_axis',(0.,1.,0.));
#12176=DIRECTION('ref_axis',(1.,0.,0.));
#12177=DIRECTION('axis',(0.,0.,1.));
#12178=DIRECTION('refdir',(1.,0.,0.));
#12179=DIRECTION('center_axis',(0.,1.,0.));
#12180=DIRECTION('ref_axis',(1.,0.,0.));
#12181=DIRECTION('center_axis',(0.,-1.,0.));
#12182=DIRECTION('ref_axis',(1.,0.,0.));
#12183=DIRECTION('',(0.,-1.,0.));
#12184=DIRECTION('center_axis',(0.,-1.,0.));
#12185=DIRECTION('ref_axis',(1.,0.,0.));
#12186=DIRECTION('center_axis',(0.,1.,0.));
#12187=DIRECTION('ref_axis',(1.,0.,0.));
#12188=DIRECTION('center_axis',(0.,1.,0.));
#12189=DIRECTION('ref_axis',(1.,0.,0.));
#12190=DIRECTION('',(0.,-1.,0.));
#12191=DIRECTION('center_axis',(0.,1.,0.));
#12192=DIRECTION('ref_axis',(1.,0.,0.));
#12193=DIRECTION('center_axis',(0.,1.,0.));
#12194=DIRECTION('ref_axis',(1.,0.,0.));
#12195=DIRECTION('center_axis',(0.,1.,0.));
#12196=DIRECTION('ref_axis',(1.,0.,0.));
#12197=DIRECTION('axis',(0.,0.,1.));
#12198=DIRECTION('refdir',(1.,0.,0.));
#12199=DIRECTION('center_axis',(0.866025403784439,0.,-0.5));
#12200=DIRECTION('ref_axis',(0.5,0.,0.866025403784439));
#12201=DIRECTION('',(-0.5,0.,-0.866025403784439));
#12202=DIRECTION('',(0.,-1.,0.));
#12203=DIRECTION('',(0.5,0.,0.866025403784439));
#12204=DIRECTION('',(0.,-1.,0.));
#12205=DIRECTION('center_axis',(1.20185167898973E-16,0.,-1.));
#12206=DIRECTION('ref_axis',(1.,0.,1.20185167898973E-16));
#12207=DIRECTION('',(-1.,0.,-1.20185167898973E-16));
#12208=DIRECTION('',(0.,-1.,0.));
#12209=DIRECTION('',(1.,0.,1.20185167898973E-16));
#12210=DIRECTION('center_axis',(-0.866025403784439,0.,-0.5));
#12211=DIRECTION('ref_axis',(0.5,0.,-0.866025403784439));
#12212=DIRECTION('',(-0.5,0.,0.866025403784439));
#12213=DIRECTION('',(0.,-1.,0.));
#12214=DIRECTION('',(0.5,0.,-0.866025403784439));
#12215=DIRECTION('center_axis',(-0.866025403784439,0.,0.5));
#12216=DIRECTION('ref_axis',(-0.5,0.,-0.866025403784439));
#12217=DIRECTION('',(0.5,0.,0.866025403784439));
#12218=DIRECTION('',(0.,-1.,0.));
#12219=DIRECTION('',(-0.5,0.,-0.866025403784439));
#12220=DIRECTION('center_axis',(-2.40370335797945E-16,0.,1.));
#12221=DIRECTION('ref_axis',(-1.,0.,-2.40370335797945E-16));
#12222=DIRECTION('',(1.,0.,2.40370335797945E-16));
#12223=DIRECTION('',(0.,-1.,0.));
#12224=DIRECTION('',(-1.,0.,-2.40370335797945E-16));
#12225=DIRECTION('center_axis',(0.866025403784439,0.,0.5));
#12226=DIRECTION('ref_axis',(-0.5,0.,0.866025403784439));
#12227=DIRECTION('',(0.5,0.,-0.866025403784439));
#12228=DIRECTION('',(-0.5,0.,0.866025403784439));
#12229=DIRECTION('center_axis',(0.,1.,0.));
#12230=DIRECTION('ref_axis',(1.,0.,0.));
#12231=DIRECTION('center_axis',(0.,-1.,0.));
#12232=DIRECTION('ref_axis',(0.,0.,-1.));
#12233=DIRECTION('center_axis',(0.,1.,0.));
#12234=DIRECTION('ref_axis',(1.,0.,0.));
#12235=DIRECTION('center_axis',(0.,1.,0.));
#12236=DIRECTION('ref_axis',(1.,0.,0.));
#12237=DIRECTION('center_axis',(0.,1.,0.));
#12238=DIRECTION('ref_axis',(0.,0.,1.));
#12239=DIRECTION('center_axis',(0.,-1.,0.));
#12240=DIRECTION('ref_axis',(1.,0.,0.));
#12241=DIRECTION('center_axis',(0.,-1.,0.));
#12242=DIRECTION('ref_axis',(1.,0.,0.));
#12243=DIRECTION('center_axis',(0.,-1.,0.));
#12244=DIRECTION('ref_axis',(1.,0.,0.));
#12245=DIRECTION('',(0.707106781186548,0.707106781186547,8.65956056235493E-17));
#12246=DIRECTION('center_axis',(0.,-1.,0.));
#12247=DIRECTION('ref_axis',(1.,0.,0.));
#12248=DIRECTION('center_axis',(0.,-1.,0.));
#12249=DIRECTION('ref_axis',(1.,0.,0.));
#12250=DIRECTION('',(0.,1.,0.));
#12251=DIRECTION('center_axis',(0.,1.,0.));
#12252=DIRECTION('ref_axis',(1.,0.,0.));
#12253=DIRECTION('center_axis',(0.,-1.,0.));
#12254=DIRECTION('ref_axis',(1.,0.,0.));
#12255=DIRECTION('',(-0.707106781186547,0.707106781186548,-8.65956056235493E-17));
#12256=DIRECTION('center_axis',(0.,-1.,0.));
#12257=DIRECTION('ref_axis',(0.,0.,-1.));
#12258=DIRECTION('center_axis',(0.,-1.,0.));
#12259=DIRECTION('ref_axis',(1.,0.,0.));
#12260=DIRECTION('center_axis',(0.,1.,0.));
#12261=DIRECTION('ref_axis',(1.,0.,0.));
#12262=DIRECTION('center_axis',(0.,1.,0.));
#12263=DIRECTION('ref_axis',(1.,0.,0.));
#12264=DIRECTION('',(-0.447213595499958,0.894427190999916,-5.47678698264203E-17));
#12265=DIRECTION('center_axis',(0.,-1.,0.));
#12266=DIRECTION('ref_axis',(1.,0.,0.));
#12267=DIRECTION('',(0.,1.,0.));
#12268=DIRECTION('axis',(0.,0.,1.));
#12269=DIRECTION('refdir',(1.,0.,0.));
#12270=DIRECTION('center_axis',(0.866025403784439,0.,-0.5));
#12271=DIRECTION('ref_axis',(0.5,0.,0.866025403784439));
#12272=DIRECTION('',(-0.5,0.,-0.866025403784439));
#12273=DIRECTION('',(0.,-1.,0.));
#12274=DIRECTION('',(0.5,0.,0.866025403784439));
#12275=DIRECTION('',(0.,-1.,0.));
#12276=DIRECTION('center_axis',(1.60246890531964E-16,0.,-1.));
#12277=DIRECTION('ref_axis',(1.,0.,1.60246890531964E-16));
#12278=DIRECTION('',(-1.,0.,-1.60246890531964E-16));
#12279=DIRECTION('',(0.,-1.,0.));
#12280=DIRECTION('',(1.,0.,1.60246890531964E-16));
#12281=DIRECTION('center_axis',(-0.866025403784439,0.,-0.5));
#12282=DIRECTION('ref_axis',(0.5,0.,-0.866025403784439));
#12283=DIRECTION('',(-0.5,0.,0.866025403784439));
#12284=DIRECTION('',(0.,-1.,0.));
#12285=DIRECTION('',(0.5,0.,-0.866025403784439));
#12286=DIRECTION('center_axis',(-0.866025403784439,0.,0.5));
#12287=DIRECTION('ref_axis',(-0.5,0.,-0.866025403784439));
#12288=DIRECTION('',(0.5,0.,0.866025403784439));
#12289=DIRECTION('',(0.,-1.,0.));
#12290=DIRECTION('',(-0.5,0.,-0.866025403784439));
#12291=DIRECTION('center_axis',(-1.60246890531964E-16,0.,1.));
#12292=DIRECTION('ref_axis',(-1.,0.,-1.60246890531964E-16));
#12293=DIRECTION('',(1.,0.,1.60246890531964E-16));
#12294=DIRECTION('',(0.,-1.,0.));
#12295=DIRECTION('',(-1.,0.,-1.60246890531964E-16));
#12296=DIRECTION('center_axis',(0.866025403784439,0.,0.5));
#12297=DIRECTION('ref_axis',(-0.5,0.,0.866025403784439));
#12298=DIRECTION('',(0.5,0.,-0.866025403784439));
#12299=DIRECTION('',(-0.5,0.,0.866025403784439));
#12300=DIRECTION('center_axis',(0.,1.,0.));
#12301=DIRECTION('ref_axis',(1.,0.,0.));
#12302=DIRECTION('center_axis',(0.,-1.,0.));
#12303=DIRECTION('ref_axis',(0.,0.,-1.));
#12304=DIRECTION('center_axis',(0.,1.,0.));
#12305=DIRECTION('ref_axis',(1.,0.,0.));
#12306=DIRECTION('center_axis',(0.,1.,0.));
#12307=DIRECTION('ref_axis',(1.,0.,0.));
#12308=DIRECTION('center_axis',(0.,1.,0.));
#12309=DIRECTION('ref_axis',(0.,0.,1.));
#12310=DIRECTION('center_axis',(0.,-1.,0.));
#12311=DIRECTION('ref_axis',(1.,0.,0.));
#12312=DIRECTION('center_axis',(0.,-1.,0.));
#12313=DIRECTION('ref_axis',(1.,0.,0.));
#12314=DIRECTION('center_axis',(0.,-1.,0.));
#12315=DIRECTION('ref_axis',(1.,0.,0.));
#12316=DIRECTION('',(0.707106781186547,0.707106781186548,8.65956056235493E-17));
#12317=DIRECTION('center_axis',(0.,-1.,0.));
#12318=DIRECTION('ref_axis',(1.,0.,0.));
#12319=DIRECTION('center_axis',(0.,-1.,0.));
#12320=DIRECTION('ref_axis',(1.,0.,0.));
#12321=DIRECTION('',(0.,1.,0.));
#12322=DIRECTION('center_axis',(0.,1.,0.));
#12323=DIRECTION('ref_axis',(1.,0.,0.));
#12324=DIRECTION('center_axis',(0.,-1.,0.));
#12325=DIRECTION('ref_axis',(1.,0.,0.));
#12326=DIRECTION('',(-0.707106781186547,0.707106781186548,-8.65956056235493E-17));
#12327=DIRECTION('center_axis',(0.,-1.,0.));
#12328=DIRECTION('ref_axis',(0.,0.,-1.));
#12329=DIRECTION('center_axis',(0.,-1.,0.));
#12330=DIRECTION('ref_axis',(1.,0.,0.));
#12331=DIRECTION('center_axis',(0.,1.,0.));
#12332=DIRECTION('ref_axis',(1.,0.,0.));
#12333=DIRECTION('center_axis',(0.,1.,0.));
#12334=DIRECTION('ref_axis',(1.,0.,0.));
#12335=DIRECTION('',(-0.447213595499958,0.894427190999916,-5.47678698264203E-17));
#12336=DIRECTION('center_axis',(0.,-1.,0.));
#12337=DIRECTION('ref_axis',(1.,0.,0.));
#12338=DIRECTION('',(0.,1.,0.));
#12339=DIRECTION('',(0.,0.,1.));
#12340=DIRECTION('',(1.,0.,0.));
#12341=DIRECTION('',(0.,0.,1.));
#12342=DIRECTION('',(1.,0.,0.));
#12343=DIRECTION('',(0.,0.,1.));
#12344=DIRECTION('',(1.,0.,0.));
#12345=DIRECTION('',(0.,0.,1.));
#12346=DIRECTION('',(1.,0.,0.));
#12347=DIRECTION('',(0.,0.,1.));
#12348=DIRECTION('',(1.,0.,0.));
#12349=DIRECTION('',(0.,-1.,2.22044604925031E-16));
#12350=DIRECTION('',(1.,0.,0.));
#12351=DIRECTION('',(0.,-1.,2.22044604925031E-16));
#12352=DIRECTION('',(1.,0.,0.));
#12353=DIRECTION('',(0.,-1.,2.22044604925031E-16));
#12354=DIRECTION('',(1.,0.,0.));
#12355=DIRECTION('',(0.,-1.,2.22044604925031E-16));
#12356=DIRECTION('',(1.,0.,0.));
#12357=DIRECTION('',(0.,0.,1.));
#12358=DIRECTION('',(1.,0.,0.));
#12359=DIRECTION('',(0.,0.,1.));
#12360=DIRECTION('',(1.,0.,0.));
#12361=DIRECTION('',(0.,0.,1.));
#12362=DIRECTION('',(1.,0.,0.));
#12363=DIRECTION('',(0.,0.,1.));
#12364=DIRECTION('',(1.,0.,0.));
#12365=DIRECTION('',(0.,0.,1.));
#12366=DIRECTION('',(1.,0.,0.));
#12367=DIRECTION('',(0.,0.,1.));
#12368=DIRECTION('',(1.,0.,0.));
#12369=DIRECTION('',(0.,-1.,2.22044604925031E-16));
#12370=DIRECTION('',(1.,0.,0.));
#12371=DIRECTION('',(0.,-1.,2.22044604925031E-16));
#12372=DIRECTION('',(1.,0.,0.));
#12373=DIRECTION('',(0.,-1.,2.22044604925031E-16));
#12374=DIRECTION('',(1.,0.,0.));
#12375=DIRECTION('',(0.,-1.,2.22044604925031E-16));
#12376=DIRECTION('',(1.,0.,0.));
#12377=DIRECTION('',(0.,0.,1.));
#12378=DIRECTION('',(1.,0.,0.));
#12379=DIRECTION('',(0.,0.,1.));
#12380=DIRECTION('',(1.,0.,0.));
#12381=DIRECTION('',(0.,0.,1.));
#12382=DIRECTION('',(1.,0.,0.));
#12383=DIRECTION('',(0.,0.,1.));
#12384=DIRECTION('',(1.,0.,0.));
#12385=DIRECTION('',(0.,0.,1.));
#12386=DIRECTION('',(1.,0.,0.));
#12387=DIRECTION('',(0.,0.,1.));
#12388=DIRECTION('',(1.,0.,0.));
#12389=DIRECTION('',(0.,-1.,2.22044604925031E-16));
#12390=DIRECTION('',(1.,0.,0.));
#12391=DIRECTION('',(0.,-1.,2.22044604925031E-16));
#12392=DIRECTION('',(1.,0.,0.));
#12393=DIRECTION('',(0.,-1.,2.22044604925031E-16));
#12394=DIRECTION('',(1.,0.,0.));
#12395=DIRECTION('',(0.,-1.,2.22044604925031E-16));
#12396=DIRECTION('',(1.,0.,0.));
#12397=DIRECTION('',(0.,0.,1.));
#12398=DIRECTION('',(1.,0.,0.));
#12399=DIRECTION('',(0.,0.,1.));
#12400=DIRECTION('',(1.,0.,0.));
#12401=DIRECTION('',(0.,0.,1.));
#12402=DIRECTION('',(1.,0.,0.));
#12403=DIRECTION('',(0.,0.,1.));
#12404=DIRECTION('',(1.,0.,0.));
#12405=DIRECTION('',(0.,0.,1.));
#12406=DIRECTION('',(1.,0.,0.));
#12407=DIRECTION('',(0.,0.,1.));
#12408=DIRECTION('',(1.,0.,0.));
#12409=DIRECTION('',(0.,-1.,2.22044604925031E-16));
#12410=DIRECTION('',(1.,0.,0.));
#12411=DIRECTION('',(0.,-1.,2.22044604925031E-16));
#12412=DIRECTION('',(1.,0.,0.));
#12413=DIRECTION('',(0.,-1.,2.22044604925031E-16));
#12414=DIRECTION('',(1.,0.,0.));
#12415=DIRECTION('',(0.,-1.,2.22044604925031E-16));
#12416=DIRECTION('',(1.,0.,0.));
#12417=DIRECTION('',(0.,0.,1.));
#12418=DIRECTION('',(1.,0.,0.));
#12419=DIRECTION('axis',(0.,0.,1.));
#12420=DIRECTION('refdir',(1.,0.,0.));
#12421=DIRECTION('axis',(0.,0.,1.));
#12422=DIRECTION('refdir',(1.,0.,0.));
#12423=DIRECTION('center_axis',(0.,1.,0.));
#12424=DIRECTION('ref_axis',(1.,0.,0.));
#12425=DIRECTION('center_axis',(0.,-1.,0.));
#12426=DIRECTION('ref_axis',(1.,0.,0.));
#12427=DIRECTION('',(0.,-1.,0.));
#12428=DIRECTION('center_axis',(0.,-1.,0.));
#12429=DIRECTION('ref_axis',(1.,0.,0.));
#12430=DIRECTION('center_axis',(0.,1.,0.));
#12431=DIRECTION('ref_axis',(1.,0.,0.));
#12432=DIRECTION('center_axis',(0.,1.,0.));
#12433=DIRECTION('ref_axis',(1.,0.,0.));
#12434=DIRECTION('',(0.,-1.,0.));
#12435=DIRECTION('center_axis',(0.,1.,0.));
#12436=DIRECTION('ref_axis',(1.,0.,0.));
#12437=DIRECTION('center_axis',(0.,1.,0.));
#12438=DIRECTION('ref_axis',(1.,0.,0.));
#12439=DIRECTION('center_axis',(0.,1.,0.));
#12440=DIRECTION('ref_axis',(1.,0.,0.));
#12441=DIRECTION('axis',(0.,0.,1.));
#12442=DIRECTION('refdir',(1.,0.,0.));
#12443=DIRECTION('center_axis',(0.,1.,0.));
#12444=DIRECTION('ref_axis',(1.,0.,0.));
#12445=DIRECTION('center_axis',(0.,-1.,0.));
#12446=DIRECTION('ref_axis',(1.,0.,0.));
#12447=DIRECTION('',(0.,-1.,0.));
#12448=DIRECTION('center_axis',(0.,-1.,0.));
#12449=DIRECTION('ref_axis',(1.,0.,0.));
#12450=DIRECTION('center_axis',(0.,1.,0.));
#12451=DIRECTION('ref_axis',(1.,0.,0.));
#12452=DIRECTION('center_axis',(0.,1.,0.));
#12453=DIRECTION('ref_axis',(1.,0.,0.));
#12454=DIRECTION('',(0.,-1.,0.));
#12455=DIRECTION('center_axis',(0.,1.,0.));
#12456=DIRECTION('ref_axis',(1.,0.,0.));
#12457=DIRECTION('center_axis',(0.,1.,0.));
#12458=DIRECTION('ref_axis',(1.,0.,0.));
#12459=DIRECTION('center_axis',(0.,1.,0.));
#12460=DIRECTION('ref_axis',(1.,0.,0.));
#12461=DIRECTION('axis',(0.,0.,1.));
#12462=DIRECTION('refdir',(1.,0.,0.));
#12463=DIRECTION('center_axis',(0.,1.,0.));
#12464=DIRECTION('ref_axis',(1.,0.,0.));
#12465=DIRECTION('center_axis',(0.,-1.,0.));
#12466=DIRECTION('ref_axis',(1.,0.,0.));
#12467=DIRECTION('',(0.,-1.,0.));
#12468=DIRECTION('center_axis',(0.,-1.,0.));
#12469=DIRECTION('ref_axis',(1.,0.,0.));
#12470=DIRECTION('center_axis',(0.,1.,0.));
#12471=DIRECTION('ref_axis',(1.,0.,0.));
#12472=DIRECTION('center_axis',(0.,1.,0.));
#12473=DIRECTION('ref_axis',(1.,0.,0.));
#12474=DIRECTION('',(0.,-1.,0.));
#12475=DIRECTION('center_axis',(0.,1.,0.));
#12476=DIRECTION('ref_axis',(1.,0.,0.));
#12477=DIRECTION('center_axis',(0.,1.,0.));
#12478=DIRECTION('ref_axis',(1.,0.,0.));
#12479=DIRECTION('center_axis',(0.,1.,0.));
#12480=DIRECTION('ref_axis',(1.,0.,0.));
#12481=DIRECTION('axis',(0.,0.,1.));
#12482=DIRECTION('refdir',(1.,0.,0.));
#12483=DIRECTION('axis',(0.,0.,1.));
#12484=DIRECTION('refdir',(1.,0.,0.));
#12485=DIRECTION('center_axis',(0.,1.,0.));
#12486=DIRECTION('ref_axis',(1.,0.,0.));
#12487=DIRECTION('center_axis',(0.,-1.,0.));
#12488=DIRECTION('ref_axis',(1.,0.,0.));
#12489=DIRECTION('',(0.,-1.,0.));
#12490=DIRECTION('center_axis',(0.,-1.,0.));
#12491=DIRECTION('ref_axis',(1.,0.,0.));
#12492=DIRECTION('center_axis',(0.,1.,0.));
#12493=DIRECTION('ref_axis',(1.,0.,0.));
#12494=DIRECTION('center_axis',(0.,1.,0.));
#12495=DIRECTION('ref_axis',(1.,0.,0.));
#12496=DIRECTION('',(0.,-1.,0.));
#12497=DIRECTION('center_axis',(0.,1.,0.));
#12498=DIRECTION('ref_axis',(1.,0.,0.));
#12499=DIRECTION('center_axis',(0.,1.,0.));
#12500=DIRECTION('ref_axis',(1.,0.,0.));
#12501=DIRECTION('center_axis',(0.,1.,0.));
#12502=DIRECTION('ref_axis',(1.,0.,0.));
#12503=DIRECTION('axis',(0.,0.,1.));
#12504=DIRECTION('refdir',(1.,0.,0.));
#12505=DIRECTION('center_axis',(0.,1.,0.));
#12506=DIRECTION('ref_axis',(1.,0.,0.));
#12507=DIRECTION('center_axis',(0.,-1.,0.));
#12508=DIRECTION('ref_axis',(1.,0.,0.));
#12509=DIRECTION('',(0.,-1.,0.));
#12510=DIRECTION('center_axis',(0.,-1.,0.));
#12511=DIRECTION('ref_axis',(1.,0.,0.));
#12512=DIRECTION('center_axis',(0.,1.,0.));
#12513=DIRECTION('ref_axis',(1.,0.,0.));
#12514=DIRECTION('center_axis',(0.,1.,0.));
#12515=DIRECTION('ref_axis',(1.,0.,0.));
#12516=DIRECTION('',(0.,-1.,0.));
#12517=DIRECTION('center_axis',(0.,1.,0.));
#12518=DIRECTION('ref_axis',(1.,0.,0.));
#12519=DIRECTION('center_axis',(0.,1.,0.));
#12520=DIRECTION('ref_axis',(1.,0.,0.));
#12521=DIRECTION('center_axis',(0.,1.,0.));
#12522=DIRECTION('ref_axis',(1.,0.,0.));
#12523=DIRECTION('axis',(0.,0.,1.));
#12524=DIRECTION('refdir',(1.,0.,0.));
#12525=DIRECTION('center_axis',(0.,1.,0.));
#12526=DIRECTION('ref_axis',(1.,0.,0.));
#12527=DIRECTION('center_axis',(0.,-1.,0.));
#12528=DIRECTION('ref_axis',(1.,0.,0.));
#12529=DIRECTION('',(0.,-1.,0.));
#12530=DIRECTION('center_axis',(0.,-1.,0.));
#12531=DIRECTION('ref_axis',(1.,0.,0.));
#12532=DIRECTION('center_axis',(0.,1.,0.));
#12533=DIRECTION('ref_axis',(1.,0.,0.));
#12534=DIRECTION('center_axis',(0.,1.,0.));
#12535=DIRECTION('ref_axis',(1.,0.,0.));
#12536=DIRECTION('',(0.,-1.,0.));
#12537=DIRECTION('center_axis',(0.,1.,0.));
#12538=DIRECTION('ref_axis',(1.,0.,0.));
#12539=DIRECTION('center_axis',(0.,1.,0.));
#12540=DIRECTION('ref_axis',(1.,0.,0.));
#12541=DIRECTION('center_axis',(0.,1.,0.));
#12542=DIRECTION('ref_axis',(1.,0.,0.));
#12543=DIRECTION('axis',(0.,0.,1.));
#12544=DIRECTION('refdir',(1.,0.,0.));
#12545=DIRECTION('axis',(0.,0.,1.));
#12546=DIRECTION('refdir',(1.,0.,0.));
#12547=DIRECTION('center_axis',(0.,1.,0.));
#12548=DIRECTION('ref_axis',(1.,0.,0.));
#12549=DIRECTION('center_axis',(0.,-1.,0.));
#12550=DIRECTION('ref_axis',(1.,0.,0.));
#12551=DIRECTION('',(0.,-1.,0.));
#12552=DIRECTION('center_axis',(0.,-1.,0.));
#12553=DIRECTION('ref_axis',(1.,0.,0.));
#12554=DIRECTION('center_axis',(0.,1.,0.));
#12555=DIRECTION('ref_axis',(1.,0.,0.));
#12556=DIRECTION('center_axis',(0.,1.,0.));
#12557=DIRECTION('ref_axis',(1.,0.,0.));
#12558=DIRECTION('',(0.,-1.,0.));
#12559=DIRECTION('center_axis',(0.,1.,0.));
#12560=DIRECTION('ref_axis',(1.,0.,0.));
#12561=DIRECTION('center_axis',(0.,1.,0.));
#12562=DIRECTION('ref_axis',(1.,0.,0.));
#12563=DIRECTION('center_axis',(0.,1.,0.));
#12564=DIRECTION('ref_axis',(1.,0.,0.));
#12565=DIRECTION('axis',(0.,0.,1.));
#12566=DIRECTION('refdir',(1.,0.,0.));
#12567=DIRECTION('center_axis',(0.,1.,0.));
#12568=DIRECTION('ref_axis',(1.,0.,0.));
#12569=DIRECTION('center_axis',(0.,-1.,0.));
#12570=DIRECTION('ref_axis',(1.,0.,0.));
#12571=DIRECTION('',(0.,-1.,0.));
#12572=DIRECTION('center_axis',(0.,-1.,0.));
#12573=DIRECTION('ref_axis',(1.,0.,0.));
#12574=DIRECTION('center_axis',(0.,1.,0.));
#12575=DIRECTION('ref_axis',(1.,0.,0.));
#12576=DIRECTION('center_axis',(0.,1.,0.));
#12577=DIRECTION('ref_axis',(1.,0.,0.));
#12578=DIRECTION('',(0.,-1.,0.));
#12579=DIRECTION('center_axis',(0.,1.,0.));
#12580=DIRECTION('ref_axis',(1.,0.,0.));
#12581=DIRECTION('center_axis',(0.,1.,0.));
#12582=DIRECTION('ref_axis',(1.,0.,0.));
#12583=DIRECTION('center_axis',(0.,1.,0.));
#12584=DIRECTION('ref_axis',(1.,0.,0.));
#12585=DIRECTION('axis',(0.,0.,1.));
#12586=DIRECTION('refdir',(1.,0.,0.));
#12587=DIRECTION('center_axis',(0.,1.,0.));
#12588=DIRECTION('ref_axis',(1.,0.,0.));
#12589=DIRECTION('center_axis',(0.,-1.,0.));
#12590=DIRECTION('ref_axis',(1.,0.,0.));
#12591=DIRECTION('',(0.,-1.,0.));
#12592=DIRECTION('center_axis',(0.,-1.,0.));
#12593=DIRECTION('ref_axis',(1.,0.,0.));
#12594=DIRECTION('center_axis',(0.,1.,0.));
#12595=DIRECTION('ref_axis',(1.,0.,0.));
#12596=DIRECTION('center_axis',(0.,1.,0.));
#12597=DIRECTION('ref_axis',(1.,0.,0.));
#12598=DIRECTION('',(0.,-1.,0.));
#12599=DIRECTION('center_axis',(0.,1.,0.));
#12600=DIRECTION('ref_axis',(1.,0.,0.));
#12601=DIRECTION('center_axis',(0.,1.,0.));
#12602=DIRECTION('ref_axis',(1.,0.,0.));
#12603=DIRECTION('center_axis',(0.,1.,0.));
#12604=DIRECTION('ref_axis',(1.,0.,0.));
#12605=DIRECTION('axis',(0.,0.,1.));
#12606=DIRECTION('refdir',(1.,0.,0.));
#12607=DIRECTION('axis',(0.,0.,1.));
#12608=DIRECTION('refdir',(1.,0.,0.));
#12609=DIRECTION('center_axis',(0.,1.,0.));
#12610=DIRECTION('ref_axis',(1.,0.,0.));
#12611=DIRECTION('center_axis',(0.,-1.,0.));
#12612=DIRECTION('ref_axis',(1.,0.,0.));
#12613=DIRECTION('',(0.,-1.,0.));
#12614=DIRECTION('center_axis',(0.,-1.,0.));
#12615=DIRECTION('ref_axis',(1.,0.,0.));
#12616=DIRECTION('center_axis',(0.,1.,0.));
#12617=DIRECTION('ref_axis',(1.,0.,0.));
#12618=DIRECTION('center_axis',(0.,1.,0.));
#12619=DIRECTION('ref_axis',(1.,0.,0.));
#12620=DIRECTION('',(0.,-1.,0.));
#12621=DIRECTION('center_axis',(0.,1.,0.));
#12622=DIRECTION('ref_axis',(1.,0.,0.));
#12623=DIRECTION('center_axis',(0.,1.,0.));
#12624=DIRECTION('ref_axis',(1.,0.,0.));
#12625=DIRECTION('center_axis',(0.,1.,0.));
#12626=DIRECTION('ref_axis',(1.,0.,0.));
#12627=DIRECTION('axis',(0.,0.,1.));
#12628=DIRECTION('refdir',(1.,0.,0.));
#12629=DIRECTION('center_axis',(0.,1.,0.));
#12630=DIRECTION('ref_axis',(1.,0.,0.));
#12631=DIRECTION('center_axis',(0.,-1.,0.));
#12632=DIRECTION('ref_axis',(1.,0.,0.));
#12633=DIRECTION('',(0.,-1.,0.));
#12634=DIRECTION('center_axis',(0.,-1.,0.));
#12635=DIRECTION('ref_axis',(1.,0.,0.));
#12636=DIRECTION('center_axis',(0.,1.,0.));
#12637=DIRECTION('ref_axis',(1.,0.,0.));
#12638=DIRECTION('center_axis',(0.,1.,0.));
#12639=DIRECTION('ref_axis',(1.,0.,0.));
#12640=DIRECTION('',(0.,-1.,0.));
#12641=DIRECTION('center_axis',(0.,1.,0.));
#12642=DIRECTION('ref_axis',(1.,0.,0.));
#12643=DIRECTION('center_axis',(0.,1.,0.));
#12644=DIRECTION('ref_axis',(1.,0.,0.));
#12645=DIRECTION('center_axis',(0.,1.,0.));
#12646=DIRECTION('ref_axis',(1.,0.,0.));
#12647=DIRECTION('axis',(0.,0.,1.));
#12648=DIRECTION('refdir',(1.,0.,0.));
#12649=DIRECTION('center_axis',(0.,1.,0.));
#12650=DIRECTION('ref_axis',(1.,0.,0.));
#12651=DIRECTION('center_axis',(0.,-1.,0.));
#12652=DIRECTION('ref_axis',(1.,0.,0.));
#12653=DIRECTION('',(0.,-1.,0.));
#12654=DIRECTION('center_axis',(0.,-1.,0.));
#12655=DIRECTION('ref_axis',(1.,0.,0.));
#12656=DIRECTION('center_axis',(0.,1.,0.));
#12657=DIRECTION('ref_axis',(1.,0.,0.));
#12658=DIRECTION('center_axis',(0.,1.,0.));
#12659=DIRECTION('ref_axis',(1.,0.,0.));
#12660=DIRECTION('',(0.,-1.,0.));
#12661=DIRECTION('center_axis',(0.,1.,0.));
#12662=DIRECTION('ref_axis',(1.,0.,0.));
#12663=DIRECTION('center_axis',(0.,1.,0.));
#12664=DIRECTION('ref_axis',(1.,0.,0.));
#12665=DIRECTION('center_axis',(0.,1.,0.));
#12666=DIRECTION('ref_axis',(1.,0.,0.));
#12667=DIRECTION('axis',(0.,0.,1.));
#12668=DIRECTION('refdir',(1.,0.,0.));
#12669=DIRECTION('axis',(0.,0.,1.));
#12670=DIRECTION('refdir',(1.,0.,0.));
#12671=DIRECTION('center_axis',(0.,-1.,0.));
#12672=DIRECTION('ref_axis',(0.,0.,-1.));
#12673=DIRECTION('center_axis',(0.,-1.,0.));
#12674=DIRECTION('ref_axis',(1.,0.,0.));
#12675=DIRECTION('center_axis',(0.,-1.,0.));
#12676=DIRECTION('ref_axis',(1.,0.,0.));
#12677=DIRECTION('center_axis',(1.,0.,1.22464679914735E-16));
#12678=DIRECTION('ref_axis',(-1.22464679914735E-16,0.,1.));
#12679=DIRECTION('center_axis',(0.,1.,0.));
#12680=DIRECTION('ref_axis',(1.,0.,0.));
#12681=DIRECTION('center_axis',(0.,1.,0.));
#12682=DIRECTION('ref_axis',(1.,0.,0.));
#12683=DIRECTION('center_axis',(0.,-1.,0.));
#12684=DIRECTION('ref_axis',(1.,0.,0.));
#12685=DIRECTION('',(0.,1.,0.));
#12686=DIRECTION('center_axis',(0.,-1.,0.));
#12687=DIRECTION('ref_axis',(1.,0.,0.));
#12688=DIRECTION('center_axis',(0.,-1.,0.));
#12689=DIRECTION('ref_axis',(1.,0.,0.));
#12690=DIRECTION('center_axis',(0.,-1.,0.));
#12691=DIRECTION('ref_axis',(1.,0.,0.));
#12692=DIRECTION('',(0.,1.,0.));
#12693=DIRECTION('center_axis',(0.,-1.,0.));
#12694=DIRECTION('ref_axis',(1.,0.,0.));
#12695=DIRECTION('center_axis',(0.,1.,0.));
#12696=DIRECTION('ref_axis',(1.,0.,0.));
#12697=DIRECTION('',(-0.707106781186547,0.707106781186548,-8.65956056235493E-17));
#12698=DIRECTION('center_axis',(0.,-1.,0.));
#12699=DIRECTION('ref_axis',(1.,0.,0.));
#12700=DIRECTION('center_axis',(0.,1.,0.));
#12701=DIRECTION('ref_axis',(0.,0.,1.));
#12702=DIRECTION('center_axis',(0.,-1.,0.));
#12703=DIRECTION('ref_axis',(1.,0.,0.));
#12704=DIRECTION('center_axis',(0.,-1.,0.));
#12705=DIRECTION('ref_axis',(1.,0.,0.));
#12706=DIRECTION('',(0.,1.,0.));
#12707=DIRECTION('center_axis',(0.,-1.,0.));
#12708=DIRECTION('ref_axis',(0.,0.,-1.));
#12709=DIRECTION('center_axis',(0.,-1.,0.));
#12710=DIRECTION('ref_axis',(1.,0.,0.));
#12711=DIRECTION('center_axis',(0.,-1.,0.));
#12712=DIRECTION('ref_axis',(1.,0.,0.));
#12713=DIRECTION('',(0.707106781186547,0.707106781186548,8.65956056235493E-17));
#12714=DIRECTION('axis',(0.,0.,1.));
#12715=DIRECTION('refdir',(1.,0.,0.));
#12716=DIRECTION('center_axis',(0.,-1.,0.));
#12717=DIRECTION('ref_axis',(0.,0.,-1.));
#12718=DIRECTION('center_axis',(0.,-1.,0.));
#12719=DIRECTION('ref_axis',(1.,0.,0.));
#12720=DIRECTION('center_axis',(0.,-1.,0.));
#12721=DIRECTION('ref_axis',(1.,0.,0.));
#12722=DIRECTION('center_axis',(1.,0.,1.22464679914735E-16));
#12723=DIRECTION('ref_axis',(-1.22464679914735E-16,0.,1.));
#12724=DIRECTION('center_axis',(0.,1.,0.));
#12725=DIRECTION('ref_axis',(1.,0.,0.));
#12726=DIRECTION('center_axis',(0.,1.,0.));
#12727=DIRECTION('ref_axis',(1.,0.,0.));
#12728=DIRECTION('center_axis',(0.,-1.,0.));
#12729=DIRECTION('ref_axis',(1.,0.,0.));
#12730=DIRECTION('center_axis',(0.,-1.,0.));
#12731=DIRECTION('ref_axis',(1.,0.,0.));
#12732=DIRECTION('',(0.,1.,0.));
#12733=DIRECTION('center_axis',(0.,1.,0.));
#12734=DIRECTION('ref_axis',(0.,0.,1.));
#12735=DIRECTION('center_axis',(0.,-1.,0.));
#12736=DIRECTION('ref_axis',(1.,0.,0.));
#12737=DIRECTION('center_axis',(0.,-1.,0.));
#12738=DIRECTION('ref_axis',(1.,0.,0.));
#12739=DIRECTION('center_axis',(0.,-1.,0.));
#12740=DIRECTION('ref_axis',(1.,0.,0.));
#12741=DIRECTION('center_axis',(0.,-1.,0.));
#12742=DIRECTION('ref_axis',(1.,0.,0.));
#12743=DIRECTION('',(0.707106781186548,0.707106781186547,8.65956056235494E-17));
#12744=DIRECTION('center_axis',(0.,-1.,0.));
#12745=DIRECTION('ref_axis',(1.,0.,0.));
#12746=DIRECTION('center_axis',(0.,-1.,0.));
#12747=DIRECTION('ref_axis',(1.,0.,0.));
#12748=DIRECTION('',(0.,1.,0.));
#12749=DIRECTION('center_axis',(0.,1.,0.));
#12750=DIRECTION('ref_axis',(1.,0.,0.));
#12751=DIRECTION('center_axis',(0.,-1.,0.));
#12752=DIRECTION('ref_axis',(1.,0.,0.));
#12753=DIRECTION('',(-0.707106781186548,0.707106781186547,-8.65956056235494E-17));
#12754=DIRECTION('center_axis',(0.,-1.,0.));
#12755=DIRECTION('ref_axis',(0.,0.,-1.));
#12756=DIRECTION('center_axis',(0.,-1.,0.));
#12757=DIRECTION('ref_axis',(1.,0.,0.));
#12758=DIRECTION('',(0.,1.,0.));
#12759=DIRECTION('axis',(0.,0.,1.));
#12760=DIRECTION('refdir',(1.,0.,0.));
#12761=DIRECTION('center_axis',(0.,0.,1.));
#12762=DIRECTION('ref_axis',(1.,0.,0.));
#12763=DIRECTION('center_axis',(1.22464679914735E-16,-1.,0.));
#12764=DIRECTION('ref_axis',(-1.,-1.22464679914735E-16,0.));
#12765=DIRECTION('center_axis',(0.707106781186548,0.,0.707106781186548));
#12766=DIRECTION('ref_axis',(0.707106781186548,0.,-0.707106781186548));
#12767=DIRECTION('center_axis',(8.65956056235494E-17,-1.,-8.65956056235493E-17));
#12768=DIRECTION('ref_axis',(-0.707106781186547,-1.22464679914735E-16,0.707106781186547));
#12769=DIRECTION('center_axis',(1.,0.,0.));
#12770=DIRECTION('ref_axis',(6.12323399573676E-17,0.,-1.));
#12771=DIRECTION('center_axis',(7.49879891330929E-33,-1.,-1.22464679914735E-16));
#12772=DIRECTION('ref_axis',(-6.12323399573676E-17,-1.22464679914735E-16,
1.));
#12773=DIRECTION('center_axis',(0.707106781186548,0.,-0.707106781186548));
#12774=DIRECTION('ref_axis',(-0.707106781186548,0.,-0.707106781186548));
#12775=DIRECTION('center_axis',(-8.65956056235493E-17,-1.,-8.65956056235494E-17));
#12776=DIRECTION('ref_axis',(0.707106781186547,-1.22464679914735E-16,0.707106781186547));
#12777=DIRECTION('center_axis',(0.,0.,-1.));
#12778=DIRECTION('ref_axis',(-1.,0.,-1.22464679914735E-16));
#12779=DIRECTION('center_axis',(-1.22464679914735E-16,-1.,-1.49975978266186E-32));
#12780=DIRECTION('ref_axis',(1.,-1.22464679914735E-16,1.22464679914735E-16));
#12781=DIRECTION('center_axis',(-0.707106781186547,0.,-0.707106781186548));
#12782=DIRECTION('ref_axis',(-0.707106781186548,0.,0.707106781186547));
#12783=DIRECTION('center_axis',(-8.65956056235493E-17,-1.,8.65956056235493E-17));
#12784=DIRECTION('ref_axis',(0.707106781186548,-1.22464679914735E-16,-0.707106781186547));
#12785=DIRECTION('center_axis',(-1.,0.,0.));
#12786=DIRECTION('ref_axis',(-1.83697019872103E-16,0.,1.));
#12787=DIRECTION('center_axis',(-2.24963967399279E-32,-1.,1.22464679914735E-16));
#12788=DIRECTION('ref_axis',(1.83697019872103E-16,-1.22464679914735E-16,
-1.));
#12789=DIRECTION('center_axis',(-0.707106781186548,0.,0.707106781186548));
#12790=DIRECTION('ref_axis',(0.707106781186547,0.,0.707106781186548));
#12791=DIRECTION('center_axis',(8.65956056235493E-17,-1.,8.65956056235493E-17));
#12792=DIRECTION('ref_axis',(-0.707106781186547,-1.22464679914735E-16,-0.707106781186548));
#12793=DIRECTION('axis',(0.,0.,1.));
#12794=DIRECTION('refdir',(1.,0.,0.));
#12795=DIRECTION('center_axis',(0.,0.,1.));
#12796=DIRECTION('ref_axis',(1.,0.,0.));
#12797=DIRECTION('center_axis',(0.,-1.,0.));
#12798=DIRECTION('ref_axis',(0.,0.,-1.));
#12799=DIRECTION('center_axis',(0.,-1.,0.));
#12800=DIRECTION('ref_axis',(0.,0.,-1.));
#12801=DIRECTION('center_axis',(0.,1.,0.));
#12802=DIRECTION('ref_axis',(1.,0.,0.));
#12803=DIRECTION('center_axis',(0.,1.,0.));
#12804=DIRECTION('ref_axis',(1.,0.,0.));
#12805=DIRECTION('center_axis',(0.,1.,0.));
#12806=DIRECTION('ref_axis',(1.,0.,0.));
#12807=DIRECTION('center_axis',(0.,1.,0.));
#12808=DIRECTION('ref_axis',(1.,0.,0.));
#12809=DIRECTION('',(0.,-1.,0.));
#12810=DIRECTION('center_axis',(0.,-1.,0.));
#12811=DIRECTION('ref_axis',(1.,0.,0.));
#12812=DIRECTION('center_axis',(0.,1.,0.));
#12813=DIRECTION('ref_axis',(1.,0.,0.));
#12814=DIRECTION('center_axis',(0.,1.,0.));
#12815=DIRECTION('ref_axis',(1.,0.,0.));
#12816=DIRECTION('center_axis',(0.,1.,0.));
#12817=DIRECTION('ref_axis',(1.,0.,0.));
#12818=DIRECTION('center_axis',(0.,1.,0.));
#12819=DIRECTION('ref_axis',(1.,0.,0.));
#12820=DIRECTION('center_axis',(0.,1.,0.));
#12821=DIRECTION('ref_axis',(1.,0.,0.));
#12822=DIRECTION('center_axis',(0.,1.,0.));
#12823=DIRECTION('ref_axis',(1.,0.,0.));
#12824=DIRECTION('center_axis',(0.,-1.,0.));
#12825=DIRECTION('ref_axis',(1.,0.,0.));
#12826=DIRECTION('center_axis',(0.,-1.,0.));
#12827=DIRECTION('ref_axis',(0.,0.,-1.));
#12828=DIRECTION('center_axis',(6.12323399573677E-17,0.,1.));
#12829=DIRECTION('ref_axis',(1.,0.,0.));
#12830=DIRECTION('center_axis',(0.,-1.,0.));
#12831=DIRECTION('ref_axis',(0.,0.,-1.));
#12832=DIRECTION('center_axis',(0.,1.,0.));
#12833=DIRECTION('ref_axis',(1.,0.,0.));
#12834=DIRECTION('center_axis',(0.,-1.,0.));
#12835=DIRECTION('ref_axis',(1.,0.,0.));
#12836=DIRECTION('center_axis',(0.,-1.,0.));
#12837=DIRECTION('ref_axis',(0.,0.,-1.));
#12838=DIRECTION('center_axis',(0.,0.,1.));
#12839=DIRECTION('ref_axis',(1.,0.,0.));
#12840=DIRECTION('center_axis',(0.,-1.,0.));
#12841=DIRECTION('ref_axis',(0.,0.,-1.));
#12842=DIRECTION('center_axis',(0.,1.,0.));
#12843=DIRECTION('ref_axis',(1.,0.,0.));
#12844=DIRECTION('center_axis',(0.,-1.,0.));
#12845=DIRECTION('ref_axis',(1.,0.,0.));
#12846=DIRECTION('center_axis',(0.,-1.,0.));
#12847=DIRECTION('ref_axis',(0.,0.,-1.));
#12848=DIRECTION('center_axis',(0.,0.,1.));
#12849=DIRECTION('ref_axis',(1.,0.,0.));
#12850=DIRECTION('center_axis',(0.,-1.,0.));
#12851=DIRECTION('ref_axis',(0.,0.,-1.));
#12852=DIRECTION('center_axis',(0.,1.,0.));
#12853=DIRECTION('ref_axis',(1.,0.,0.));
#12854=DIRECTION('center_axis',(0.,-1.,0.));
#12855=DIRECTION('ref_axis',(1.,0.,0.));
#12856=DIRECTION('center_axis',(0.,-1.,0.));
#12857=DIRECTION('ref_axis',(0.,0.,-1.));
#12858=DIRECTION('center_axis',(0.,0.,1.));
#12859=DIRECTION('ref_axis',(1.,0.,0.));
#12860=DIRECTION('center_axis',(0.,-1.,0.));
#12861=DIRECTION('ref_axis',(0.,0.,-1.));
#12862=DIRECTION('center_axis',(0.,1.,0.));
#12863=DIRECTION('ref_axis',(1.,0.,0.));
#12864=DIRECTION('center_axis',(0.,-1.,0.));
#12865=DIRECTION('ref_axis',(1.,0.,0.));
#12866=DIRECTION('center_axis',(0.,-1.,0.));
#12867=DIRECTION('ref_axis',(0.,0.,-1.));
#12868=DIRECTION('center_axis',(6.12323399573676E-17,0.,1.));
#12869=DIRECTION('ref_axis',(1.,0.,0.));
#12870=DIRECTION('center_axis',(0.,-1.,0.));
#12871=DIRECTION('ref_axis',(0.,0.,-1.));
#12872=DIRECTION('center_axis',(0.,1.,0.));
#12873=DIRECTION('ref_axis',(1.,0.,0.));
#12874=DIRECTION('center_axis',(0.,-1.,0.));
#12875=DIRECTION('ref_axis',(1.,0.,0.));
#12876=DIRECTION('center_axis',(0.,-1.,0.));
#12877=DIRECTION('ref_axis',(0.,0.,-1.));
#12878=DIRECTION('center_axis',(0.,0.,1.));
#12879=DIRECTION('ref_axis',(1.,0.,0.));
#12880=DIRECTION('center_axis',(0.,-1.,0.));
#12881=DIRECTION('ref_axis',(0.,0.,-1.));
#12882=DIRECTION('center_axis',(0.,1.,0.));
#12883=DIRECTION('ref_axis',(1.,0.,0.));
#12884=DIRECTION('center_axis',(0.,1.,0.));
#12885=DIRECTION('ref_axis',(1.,0.,0.));
#12886=DIRECTION('',(0.,1.,0.));
#12887=DIRECTION('center_axis',(0.,-1.,0.));
#12888=DIRECTION('ref_axis',(1.,0.,0.));
#12889=DIRECTION('center_axis',(0.,-1.,0.));
#12890=DIRECTION('ref_axis',(1.,0.,0.));
#12891=DIRECTION('center_axis',(0.,1.,0.));
#12892=DIRECTION('ref_axis',(1.,0.,0.));
#12893=DIRECTION('center_axis',(0.,-1.,0.));
#12894=DIRECTION('ref_axis',(0.,0.,-1.));
#12895=DIRECTION('center_axis',(0.,0.,1.));
#12896=DIRECTION('ref_axis',(1.,0.,0.));
#12897=DIRECTION('center_axis',(0.,-1.,0.));
#12898=DIRECTION('ref_axis',(0.,0.,-1.));
#12899=DIRECTION('center_axis',(0.,-1.,0.));
#12900=DIRECTION('ref_axis',(-1.,0.,0.));
#12901=DIRECTION('center_axis',(0.,1.,0.));
#12902=DIRECTION('ref_axis',(1.,0.,0.));
#12903=DIRECTION('axis',(0.,0.,1.));
#12904=DIRECTION('refdir',(1.,0.,0.));
#12905=DIRECTION('center_axis',(0.,1.,0.));
#12906=DIRECTION('ref_axis',(0.,0.,1.));
#12907=DIRECTION('center_axis',(0.,-1.,0.));
#12908=DIRECTION('ref_axis',(1.,0.,0.));
#12909=DIRECTION('center_axis',(0.,-1.,0.));
#12910=DIRECTION('ref_axis',(1.,0.,0.));
#12911=DIRECTION('center_axis',(0.,-1.,0.));
#12912=DIRECTION('ref_axis',(1.,0.,0.));
#12913=DIRECTION('center_axis',(0.,-1.,0.));
#12914=DIRECTION('ref_axis',(1.,0.,0.));
#12915=DIRECTION('',(0.,1.,0.));
#12916=DIRECTION('center_axis',(0.,-1.,0.));
#12917=DIRECTION('ref_axis',(0.,0.,-1.));
#12918=DIRECTION('center_axis',(0.,-1.,0.));
#12919=DIRECTION('ref_axis',(1.,0.,0.));
#12920=DIRECTION('center_axis',(0.,-1.,0.));
#12921=DIRECTION('ref_axis',(1.,0.,0.));
#12922=DIRECTION('',(0.,1.,0.));
#12923=DIRECTION('center_axis',(0.,1.,0.));
#12924=DIRECTION('ref_axis',(0.,0.,1.));
#12925=DIRECTION('center_axis',(0.,-1.,0.));
#12926=DIRECTION('ref_axis',(1.,0.,0.));
#12927=DIRECTION('center_axis',(0.,-1.,0.));
#12928=DIRECTION('ref_axis',(1.,0.,0.));
#12929=DIRECTION('center_axis',(0.,-1.,0.));
#12930=DIRECTION('ref_axis',(1.,0.,0.));
#12931=DIRECTION('center_axis',(0.,-1.,0.));
#12932=DIRECTION('ref_axis',(1.,0.,0.));
#12933=DIRECTION('',(0.,1.,0.));
#12934=DIRECTION('center_axis',(0.,-1.,0.));
#12935=DIRECTION('ref_axis',(0.,0.,-1.));
#12936=DIRECTION('center_axis',(0.,-1.,0.));
#12937=DIRECTION('ref_axis',(1.,0.,0.));
#12938=DIRECTION('center_axis',(0.,-1.,0.));
#12939=DIRECTION('ref_axis',(1.,0.,0.));
#12940=DIRECTION('',(0.,1.,0.));
#12941=DIRECTION('',(0.,0.,1.));
#12942=DIRECTION('',(1.,0.,0.));
#12943=DIRECTION('',(0.,0.,1.));
#12944=DIRECTION('',(1.,0.,0.));
#12945=DIRECTION('',(0.,0.,1.));
#12946=DIRECTION('',(1.,0.,0.));
#12947=DIRECTION('',(0.,0.,1.));
#12948=DIRECTION('',(1.,0.,0.));
#12949=DIRECTION('',(0.,0.,1.));
#12950=DIRECTION('',(1.,0.,0.));
#12951=DIRECTION('',(0.,0.,1.));
#12952=DIRECTION('',(1.,0.,0.));
#12953=DIRECTION('',(0.,0.,1.));
#12954=DIRECTION('',(1.,0.,0.));
#12955=DIRECTION('',(0.,0.,1.));
#12956=DIRECTION('',(1.,0.,0.));
#12957=DIRECTION('',(0.,0.,1.));
#12958=DIRECTION('',(1.,0.,0.));
#12959=DIRECTION('',(0.,0.,1.));
#12960=DIRECTION('',(1.,0.,0.));
#12961=DIRECTION('',(0.,0.,1.));
#12962=DIRECTION('',(1.,0.,0.));
#12963=DIRECTION('',(0.,0.,1.));
#12964=DIRECTION('',(1.,0.,0.));
#12965=DIRECTION('',(0.,0.,1.));
#12966=DIRECTION('',(1.,0.,0.));
#12967=DIRECTION('',(0.,0.,1.));
#12968=DIRECTION('',(1.,0.,0.));
#12969=DIRECTION('',(0.,0.,1.));
#12970=DIRECTION('',(1.,0.,0.));
#12971=DIRECTION('',(0.,0.,1.));
#12972=DIRECTION('',(1.,0.,0.));
#12973=DIRECTION('',(0.,0.,1.));
#12974=DIRECTION('',(1.,0.,0.));
#12975=DIRECTION('',(0.,0.,1.));
#12976=DIRECTION('',(1.,0.,0.));
#12977=DIRECTION('',(0.,0.,1.));
#12978=DIRECTION('',(1.,0.,0.));
#12979=DIRECTION('',(0.,0.,1.));
#12980=DIRECTION('',(1.,0.,0.));
#12981=DIRECTION('',(0.,0.,1.));
#12982=DIRECTION('',(1.,0.,0.));
#12983=DIRECTION('',(0.,0.,1.));
#12984=DIRECTION('',(1.,0.,0.));
#12985=DIRECTION('',(0.,0.,1.));
#12986=DIRECTION('',(1.,0.,0.));
#12987=DIRECTION('',(0.,0.,1.));
#12988=DIRECTION('',(1.,0.,0.));
#12989=DIRECTION('',(0.,0.,1.));
#12990=DIRECTION('',(2.22044604925031E-16,1.,0.));
#12991=DIRECTION('',(0.,0.,1.));
#12992=DIRECTION('',(-1.,1.22464679914735E-16,0.));
#12993=DIRECTION('',(0.,0.,1.));
#12994=DIRECTION('',(-2.22044604925031E-16,-1.,0.));
#12995=DIRECTION('',(0.,0.,1.));
#12996=DIRECTION('',(1.,0.,0.));
#12997=DIRECTION('',(0.,0.,1.));
#12998=DIRECTION('',(2.22044604925031E-16,1.,0.));
#12999=DIRECTION('',(0.,0.,1.));
#13000=DIRECTION('',(-1.,1.22464679914735E-16,0.));
#13001=DIRECTION('',(0.,0.,1.));
#13002=DIRECTION('',(-2.22044604925031E-16,-1.,0.));
#13003=CARTESIAN_POINT('',(0.,0.,0.));
#13004=CARTESIAN_POINT('',(0.,0.,0.));
#13005=CARTESIAN_POINT('',(0.,0.,0.));
#13006=CARTESIAN_POINT('Origin',(13.,-1.8,-0.1));
#13007=CARTESIAN_POINT('',(12.79,-1.8,0.));
#13008=CARTESIAN_POINT('Origin',(13.,-1.8,0.));
#13009=CARTESIAN_POINT('',(12.79,-1.8,1.));
#13010=CARTESIAN_POINT('',(12.79,-1.8,-0.1));
#13011=CARTESIAN_POINT('Origin',(13.,-1.8,1.));
#13012=CARTESIAN_POINT('Origin',(17.,1.8,-0.1));
#13013=CARTESIAN_POINT('',(16.79,1.8,0.));
#13014=CARTESIAN_POINT('Origin',(17.,1.8,0.));
#13015=CARTESIAN_POINT('',(16.79,1.8,1.));
#13016=CARTESIAN_POINT('',(16.79,1.8,-0.1));
#13017=CARTESIAN_POINT('Origin',(17.,1.8,1.));
#13018=CARTESIAN_POINT('Origin',(13.,1.8,-0.1));
#13019=CARTESIAN_POINT('',(12.79,1.8,0.));
#13020=CARTESIAN_POINT('Origin',(13.,1.8,0.));
#13021=CARTESIAN_POINT('',(12.79,1.8,1.));
#13022=CARTESIAN_POINT('',(12.79,1.8,-0.1));
#13023=CARTESIAN_POINT('Origin',(13.,1.8,1.));
#13024=CARTESIAN_POINT('Origin',(17.,-1.8,-0.1));
#13025=CARTESIAN_POINT('',(16.79,-1.8,0.));
#13026=CARTESIAN_POINT('Origin',(17.,-1.8,0.));
#13027=CARTESIAN_POINT('',(16.79,-1.8,1.));
#13028=CARTESIAN_POINT('',(16.79,-1.8,-0.1));
#13029=CARTESIAN_POINT('Origin',(17.,-1.8,1.));
#13030=CARTESIAN_POINT('Origin',(-1.8,-13.,-0.1));
#13031=CARTESIAN_POINT('',(-2.01,-13.,0.));
#13032=CARTESIAN_POINT('Origin',(-1.8,-13.,0.));
#13033=CARTESIAN_POINT('',(-2.01,-13.,1.));
#13034=CARTESIAN_POINT('',(-2.01,-13.,-0.1));
#13035=CARTESIAN_POINT('Origin',(-1.8,-13.,1.));
#13036=CARTESIAN_POINT('Origin',(1.8,-17.,-0.1));
#13037=CARTESIAN_POINT('',(1.59,-17.,0.));
#13038=CARTESIAN_POINT('Origin',(1.8,-17.,0.));
#13039=CARTESIAN_POINT('',(1.59,-17.,1.));
#13040=CARTESIAN_POINT('',(1.59,-17.,-0.1));
#13041=CARTESIAN_POINT('Origin',(1.8,-17.,1.));
#13042=CARTESIAN_POINT('Origin',(1.8,-13.,-0.1));
#13043=CARTESIAN_POINT('',(1.59,-13.,0.));
#13044=CARTESIAN_POINT('Origin',(1.8,-13.,0.));
#13045=CARTESIAN_POINT('',(1.59,-13.,1.));
#13046=CARTESIAN_POINT('',(1.59,-13.,-0.1));
#13047=CARTESIAN_POINT('Origin',(1.8,-13.,1.));
#13048=CARTESIAN_POINT('Origin',(-1.8,-17.,-0.1));
#13049=CARTESIAN_POINT('',(-2.01,-17.,0.));
#13050=CARTESIAN_POINT('Origin',(-1.8,-17.,0.));
#13051=CARTESIAN_POINT('',(-2.01,-17.,1.));
#13052=CARTESIAN_POINT('',(-2.01,-17.,-0.1));
#13053=CARTESIAN_POINT('Origin',(-1.8,-17.,1.));
#13054=CARTESIAN_POINT('Origin',(-13.,1.8,-0.1));
#13055=CARTESIAN_POINT('',(-13.21,1.8,0.));
#13056=CARTESIAN_POINT('Origin',(-13.,1.8,0.));
#13057=CARTESIAN_POINT('',(-13.21,1.8,1.));
#13058=CARTESIAN_POINT('',(-13.21,1.8,-0.1));
#13059=CARTESIAN_POINT('Origin',(-13.,1.8,1.));
#13060=CARTESIAN_POINT('Origin',(-17.,-1.8,-0.1));
#13061=CARTESIAN_POINT('',(-17.21,-1.8,0.));
#13062=CARTESIAN_POINT('Origin',(-17.,-1.8,0.));
#13063=CARTESIAN_POINT('',(-17.21,-1.8,1.));
#13064=CARTESIAN_POINT('',(-17.21,-1.8,-0.1));
#13065=CARTESIAN_POINT('Origin',(-17.,-1.8,1.));
#13066=CARTESIAN_POINT('Origin',(-13.,-1.8,-0.1));
#13067=CARTESIAN_POINT('',(-13.21,-1.8,0.));
#13068=CARTESIAN_POINT('Origin',(-13.,-1.8,0.));
#13069=CARTESIAN_POINT('',(-13.21,-1.8,1.));
#13070=CARTESIAN_POINT('',(-13.21,-1.8,-0.1));
#13071=CARTESIAN_POINT('Origin',(-13.,-1.8,1.));
#13072=CARTESIAN_POINT('Origin',(-17.,1.8,-0.1));
#13073=CARTESIAN_POINT('',(-17.21,1.8,0.));
#13074=CARTESIAN_POINT('Origin',(-17.,1.8,0.));
#13075=CARTESIAN_POINT('',(-17.21,1.8,1.));
#13076=CARTESIAN_POINT('',(-17.21,1.8,-0.1));
#13077=CARTESIAN_POINT('Origin',(-17.,1.8,1.));
#13078=CARTESIAN_POINT('Origin',(1.8,13.,-0.1));
#13079=CARTESIAN_POINT('',(1.59,13.,0.));
#13080=CARTESIAN_POINT('Origin',(1.8,13.,0.));
#13081=CARTESIAN_POINT('',(1.59,13.,1.));
#13082=CARTESIAN_POINT('',(1.59,13.,-0.1));
#13083=CARTESIAN_POINT('Origin',(1.8,13.,1.));
#13084=CARTESIAN_POINT('Origin',(-1.8,17.,-0.1));
#13085=CARTESIAN_POINT('',(-2.01,17.,0.));
#13086=CARTESIAN_POINT('Origin',(-1.8,17.,0.));
#13087=CARTESIAN_POINT('',(-2.01,17.,1.));
#13088=CARTESIAN_POINT('',(-2.01,17.,-0.1));
#13089=CARTESIAN_POINT('Origin',(-1.8,17.,1.));
#13090=CARTESIAN_POINT('Origin',(-1.8,13.,-0.1));
#13091=CARTESIAN_POINT('',(-2.01,13.,0.));
#13092=CARTESIAN_POINT('Origin',(-1.8,13.,0.));
#13093=CARTESIAN_POINT('',(-2.01,13.,1.));
#13094=CARTESIAN_POINT('',(-2.01,13.,-0.1));
#13095=CARTESIAN_POINT('Origin',(-1.8,13.,1.));
#13096=CARTESIAN_POINT('Origin',(1.8,17.,-0.1));
#13097=CARTESIAN_POINT('',(1.59,17.,0.));
#13098=CARTESIAN_POINT('Origin',(1.8,17.,0.));
#13099=CARTESIAN_POINT('',(1.59,17.,1.));
#13100=CARTESIAN_POINT('',(1.59,17.,-0.1));
#13101=CARTESIAN_POINT('Origin',(1.8,17.,1.));
#13102=CARTESIAN_POINT('Origin',(-2.40416305603426,-2.40416305603426,-0.1));
#13103=CARTESIAN_POINT('',(-2.65416305603426,-2.40416305603426,0.));
#13104=CARTESIAN_POINT('Origin',(-2.40416305603426,-2.40416305603426,0.));
#13105=CARTESIAN_POINT('',(-2.65416305603426,-2.40416305603426,1.));
#13106=CARTESIAN_POINT('',(-2.65416305603426,-2.40416305603426,-0.1));
#13107=CARTESIAN_POINT('Origin',(-2.40416305603426,-2.40416305603426,1.));
#13108=CARTESIAN_POINT('Origin',(-2.40416305603426,2.40416305603426,-0.1));
#13109=CARTESIAN_POINT('',(-2.65416305603426,2.40416305603426,0.));
#13110=CARTESIAN_POINT('Origin',(-2.40416305603426,2.40416305603426,0.));
#13111=CARTESIAN_POINT('',(-2.65416305603426,2.40416305603426,1.));
#13112=CARTESIAN_POINT('',(-2.65416305603426,2.40416305603426,-0.1));
#13113=CARTESIAN_POINT('Origin',(-2.40416305603426,2.40416305603426,1.));
#13114=CARTESIAN_POINT('Origin',(2.40416305603426,2.40416305603426,-0.1));
#13115=CARTESIAN_POINT('',(2.15416305603426,2.40416305603426,0.));
#13116=CARTESIAN_POINT('Origin',(2.40416305603426,2.40416305603426,0.));
#13117=CARTESIAN_POINT('',(2.15416305603426,2.40416305603426,1.));
#13118=CARTESIAN_POINT('',(2.15416305603426,2.40416305603426,-0.1));
#13119=CARTESIAN_POINT('Origin',(2.40416305603426,2.40416305603426,1.));
#13120=CARTESIAN_POINT('Origin',(2.40416305603426,-2.40416305603426,-0.1));
#13121=CARTESIAN_POINT('',(2.15416305603426,-2.40416305603426,0.));
#13122=CARTESIAN_POINT('Origin',(2.40416305603426,-2.40416305603426,0.));
#13123=CARTESIAN_POINT('',(2.15416305603426,-2.40416305603426,1.));
#13124=CARTESIAN_POINT('',(2.15416305603426,-2.40416305603426,-0.1));
#13125=CARTESIAN_POINT('Origin',(2.40416305603426,-2.40416305603426,1.));
#13126=CARTESIAN_POINT('Origin',(21.,21.,0.));
#13127=CARTESIAN_POINT('',(21.,21.,0.));
#13128=CARTESIAN_POINT('',(-21.,21.,0.));
#13129=CARTESIAN_POINT('',(21.,21.,0.));
#13130=CARTESIAN_POINT('',(-21.,21.,1.));
#13131=CARTESIAN_POINT('',(-21.,21.,0.));
#13132=CARTESIAN_POINT('',(21.,21.,1.));
#13133=CARTESIAN_POINT('',(21.,21.,1.));
#13134=CARTESIAN_POINT('',(21.,21.,0.));
#13135=CARTESIAN_POINT('Origin',(21.,-21.,0.));
#13136=CARTESIAN_POINT('',(21.,-21.,0.));
#13137=CARTESIAN_POINT('',(21.,-21.,0.));
#13138=CARTESIAN_POINT('',(21.,-21.,1.));
#13139=CARTESIAN_POINT('',(21.,-21.,1.));
#13140=CARTESIAN_POINT('',(21.,-21.,0.));
#13141=CARTESIAN_POINT('Origin',(-21.,-21.,0.));
#13142=CARTESIAN_POINT('',(-21.,-21.,0.));
#13143=CARTESIAN_POINT('',(-21.,-21.,0.));
#13144=CARTESIAN_POINT('',(-21.,-21.,1.));
#13145=CARTESIAN_POINT('',(-21.,-21.,1.));
#13146=CARTESIAN_POINT('',(-21.,-21.,0.));
#13147=CARTESIAN_POINT('Origin',(-21.,21.,0.));
#13148=CARTESIAN_POINT('',(-21.,21.,0.));
#13149=CARTESIAN_POINT('',(-21.,21.,1.));
#13150=CARTESIAN_POINT('Origin',(0.,0.,1.));
#13151=CARTESIAN_POINT('Origin',(0.,0.,0.));
#13152=CARTESIAN_POINT('',(0.,0.,0.));
#13153=CARTESIAN_POINT('Origin',(2.40416305603426,-2.40416305603426,1.8));
#13154=CARTESIAN_POINT('',(1.80416305603426,-2.40416305603426,1.8));
#13155=CARTESIAN_POINT('',(1.80416305603426,-2.40416305603426,4.6));
#13156=CARTESIAN_POINT('',(1.80416305603426,-2.40416305603426,1.8));
#13157=CARTESIAN_POINT('',(2.82842712474619,-2.82842712474619,1.8));
#13158=CARTESIAN_POINT('Origin',(2.40416305603426,-2.40416305603426,1.8));
#13159=CARTESIAN_POINT('',(2.82842712474619,-2.82842712474619,4.6));
#13160=CARTESIAN_POINT('',(2.82842712474619,-2.82842712474619,1.8));
#13161=CARTESIAN_POINT('Origin',(2.40416305603426,-2.40416305603426,4.6));
#13162=CARTESIAN_POINT('Origin',(2.40416305603426,2.40416305603426,1.8));
#13163=CARTESIAN_POINT('',(1.80416305603426,2.40416305603426,1.8));
#13164=CARTESIAN_POINT('',(1.80416305603426,2.40416305603426,4.6));
#13165=CARTESIAN_POINT('',(1.80416305603426,2.40416305603426,1.8));
#13166=CARTESIAN_POINT('',(2.82842712474619,2.82842712474619,1.8));
#13167=CARTESIAN_POINT('Origin',(2.40416305603426,2.40416305603426,1.8));
#13168=CARTESIAN_POINT('',(2.82842712474619,2.82842712474619,4.6));
#13169=CARTESIAN_POINT('',(2.82842712474619,2.82842712474619,1.8));
#13170=CARTESIAN_POINT('Origin',(2.40416305603426,2.40416305603426,4.6));
#13171=CARTESIAN_POINT('Origin',(-2.40416305603426,2.40416305603426,1.8));
#13172=CARTESIAN_POINT('',(-3.00416305603426,2.40416305603426,1.8));
#13173=CARTESIAN_POINT('',(-3.00416305603426,2.40416305603426,4.6));
#13174=CARTESIAN_POINT('',(-3.00416305603426,2.40416305603426,1.8));
#13175=CARTESIAN_POINT('',(-2.82842712474619,2.82842712474619,1.8));
#13176=CARTESIAN_POINT('Origin',(-2.40416305603426,2.40416305603426,1.8));
#13177=CARTESIAN_POINT('',(-2.82842712474619,2.82842712474619,4.6));
#13178=CARTESIAN_POINT('',(-2.82842712474619,2.82842712474619,1.8));
#13179=CARTESIAN_POINT('Origin',(-2.40416305603426,2.40416305603426,4.6));
#13180=CARTESIAN_POINT('Origin',(-2.40416305603426,-2.40416305603426,1.8));
#13181=CARTESIAN_POINT('',(-3.00416305603426,-2.40416305603426,1.8));
#13182=CARTESIAN_POINT('',(-3.00416305603426,-2.40416305603426,4.6));
#13183=CARTESIAN_POINT('',(-3.00416305603426,-2.40416305603426,1.8));
#13184=CARTESIAN_POINT('',(-2.82842712474619,-2.82842712474619,1.8));
#13185=CARTESIAN_POINT('Origin',(-2.40416305603426,-2.40416305603426,1.8));
#13186=CARTESIAN_POINT('',(-2.82842712474619,-2.82842712474619,4.6));
#13187=CARTESIAN_POINT('',(-2.82842712474619,-2.82842712474619,1.8));
#13188=CARTESIAN_POINT('Origin',(-2.40416305603426,-2.40416305603426,4.6));
#13189=CARTESIAN_POINT('Origin',(-3.4,4.163799117101E-16,3.4));
#13190=CARTESIAN_POINT('',(-3.565,3.96173239524169E-16,3.4));
#13191=CARTESIAN_POINT('Origin',(-3.4,4.163799117101E-16,3.4));
#13192=CARTESIAN_POINT('',(-3.565,4.36586583896031E-16,4.6));
#13193=CARTESIAN_POINT('',(-3.565,3.96173239524169E-16,3.4));
#13194=CARTESIAN_POINT('Origin',(-3.4,4.163799117101E-16,4.6));
#13195=CARTESIAN_POINT('Origin',(-3.4,4.16333634234434E-16,3.4));
#13196=CARTESIAN_POINT('Origin',(2.0818995585505E-16,3.4,3.4));
#13197=CARTESIAN_POINT('',(-0.165,3.4,3.4));
#13198=CARTESIAN_POINT('Origin',(2.0818995585505E-16,3.4,3.4));
#13199=CARTESIAN_POINT('',(-0.165,3.4,4.6));
#13200=CARTESIAN_POINT('',(-0.165,3.4,3.4));
#13201=CARTESIAN_POINT('Origin',(2.0818995585505E-16,3.4,4.6));
#13202=CARTESIAN_POINT('Origin',(2.22044604925031E-16,3.4,3.4));
#13203=CARTESIAN_POINT('Origin',(3.4,0.,3.4));
#13204=CARTESIAN_POINT('',(3.235,-2.02066721859313E-17,3.4));
#13205=CARTESIAN_POINT('Origin',(3.4,0.,3.4));
#13206=CARTESIAN_POINT('',(3.235,2.02066721859313E-17,4.6));
#13207=CARTESIAN_POINT('',(3.235,-2.02066721859313E-17,3.4));
#13208=CARTESIAN_POINT('Origin',(3.4,0.,4.6));
#13209=CARTESIAN_POINT('Origin',(3.4,0.,3.4));
#13210=CARTESIAN_POINT('Origin',(-6.2456986756515E-16,-3.4,3.4));
#13211=CARTESIAN_POINT('',(-0.165000000000001,-3.4,3.4));
#13212=CARTESIAN_POINT('Origin',(-6.2456986756515E-16,-3.4,3.4));
#13213=CARTESIAN_POINT('',(-0.165000000000001,-3.4,4.6));
#13214=CARTESIAN_POINT('',(-0.165000000000001,-3.4,3.4));
#13215=CARTESIAN_POINT('Origin',(-6.2456986756515E-16,-3.4,4.6));
#13216=CARTESIAN_POINT('Origin',(-6.38378239159465E-16,-3.4,3.4));
#13217=CARTESIAN_POINT('Origin',(-2.40416305603426,-2.40416305603426,1.8));
#13218=CARTESIAN_POINT('Origin',(-2.40416305603426,-2.40416305603426,4.6));
#13219=CARTESIAN_POINT('',(-2.82842712474619,-2.82842712474619,1.8));
#13220=CARTESIAN_POINT('Origin',(-2.40416305603426,-2.40416305603426,1.8));
#13221=CARTESIAN_POINT('Origin',(-2.40416305603426,-2.40416305603426,1.8));
#13222=CARTESIAN_POINT('',(-2.73416305603426,-2.40416305603426,1.8));
#13223=CARTESIAN_POINT('Origin',(-2.40416305603426,-2.40416305603426,1.8));
#13224=CARTESIAN_POINT('Origin',(-2.40416305603426,2.40416305603426,1.8));
#13225=CARTESIAN_POINT('Origin',(-2.40416305603426,2.40416305603426,4.6));
#13226=CARTESIAN_POINT('',(-2.82842712474619,2.82842712474619,1.8));
#13227=CARTESIAN_POINT('Origin',(-2.40416305603426,2.40416305603426,1.8));
#13228=CARTESIAN_POINT('Origin',(-2.40416305603426,2.40416305603426,1.8));
#13229=CARTESIAN_POINT('',(-2.73416305603426,2.40416305603426,1.8));
#13230=CARTESIAN_POINT('Origin',(-2.40416305603426,2.40416305603426,1.8));
#13231=CARTESIAN_POINT('Origin',(2.40416305603426,2.40416305603426,1.8));
#13232=CARTESIAN_POINT('Origin',(2.40416305603426,2.40416305603426,4.6));
#13233=CARTESIAN_POINT('',(2.82842712474619,2.82842712474619,1.8));
#13234=CARTESIAN_POINT('Origin',(2.40416305603426,2.40416305603426,1.8));
#13235=CARTESIAN_POINT('Origin',(2.40416305603426,2.40416305603426,1.8));
#13236=CARTESIAN_POINT('',(2.07416305603426,2.40416305603426,1.8));
#13237=CARTESIAN_POINT('Origin',(2.40416305603426,2.40416305603426,1.8));
#13238=CARTESIAN_POINT('Origin',(2.40416305603426,-2.40416305603426,1.8));
#13239=CARTESIAN_POINT('Origin',(2.40416305603426,-2.40416305603426,4.6));
#13240=CARTESIAN_POINT('',(2.82842712474619,-2.82842712474619,1.8));
#13241=CARTESIAN_POINT('Origin',(2.40416305603426,-2.40416305603426,1.8));
#13242=CARTESIAN_POINT('Origin',(2.40416305603426,-2.40416305603426,1.8));
#13243=CARTESIAN_POINT('',(2.07416305603426,-2.40416305603426,1.8));
#13244=CARTESIAN_POINT('Origin',(2.40416305603426,-2.40416305603426,1.8));
#13245=CARTESIAN_POINT('Origin',(0.,0.,4.6));
#13246=CARTESIAN_POINT('Origin',(0.,0.,4.6));
#13247=CARTESIAN_POINT('Origin',(0.,0.,4.6));
#13248=CARTESIAN_POINT('Origin',(0.,0.,4.6));
#13249=CARTESIAN_POINT('Origin',(0.,0.,4.6));
#13250=CARTESIAN_POINT('',(-2.6,-3.18408167778312E-16,4.6));
#13251=CARTESIAN_POINT('Origin',(0.,0.,4.6));
#13252=CARTESIAN_POINT('Origin',(-2.40416305603426,-2.40416305603426,0.9));
#13253=CARTESIAN_POINT('',(-2.73416305603426,-2.40416305603426,1.));
#13254=CARTESIAN_POINT('Origin',(-2.40416305603426,-2.40416305603426,1.));
#13255=CARTESIAN_POINT('',(-2.73416305603426,-2.40416305603426,0.9));
#13256=CARTESIAN_POINT('Origin',(-2.40416305603426,2.40416305603426,0.9));
#13257=CARTESIAN_POINT('',(-2.73416305603426,2.40416305603426,1.));
#13258=CARTESIAN_POINT('Origin',(-2.40416305603426,2.40416305603426,1.));
#13259=CARTESIAN_POINT('',(-2.73416305603426,2.40416305603426,0.9));
#13260=CARTESIAN_POINT('Origin',(2.40416305603426,2.40416305603426,0.9));
#13261=CARTESIAN_POINT('',(2.07416305603426,2.40416305603426,1.));
#13262=CARTESIAN_POINT('Origin',(2.40416305603426,2.40416305603426,1.));
#13263=CARTESIAN_POINT('',(2.07416305603426,2.40416305603426,0.9));
#13264=CARTESIAN_POINT('Origin',(2.40416305603426,-2.40416305603426,0.9));
#13265=CARTESIAN_POINT('',(2.07416305603426,-2.40416305603426,1.));
#13266=CARTESIAN_POINT('Origin',(2.40416305603426,-2.40416305603426,1.));
#13267=CARTESIAN_POINT('',(2.07416305603426,-2.40416305603426,0.9));
#13268=CARTESIAN_POINT('Origin',(0.,0.,2.75));
#13269=CARTESIAN_POINT('',(-2.6,-3.18408167778312E-16,2.75));
#13270=CARTESIAN_POINT('',(-2.6,-3.18408167778312E-16,2.75));
#13271=CARTESIAN_POINT('Origin',(0.,0.,2.75));
#13272=CARTESIAN_POINT('Origin',(0.,0.,1.));
#13273=CARTESIAN_POINT('',(-2.2,-2.69422295812418E-16,2.75));
#13274=CARTESIAN_POINT('Origin',(0.,0.,2.75));
#13275=CARTESIAN_POINT('',(-2.2,-2.69422295812418E-16,1.));
#13276=CARTESIAN_POINT('',(-2.2,-2.69422295812418E-16,1.));
#13277=CARTESIAN_POINT('Origin',(0.,0.,1.));
#13278=CARTESIAN_POINT('Origin',(0.,0.,1.));
#13279=CARTESIAN_POINT('',(-2.82842712474619,2.82842712474619,1.));
#13280=CARTESIAN_POINT('',(-2.82842712474619,2.82842712474619,1.));
#13281=CARTESIAN_POINT('Origin',(0.,0.,1.));
#13282=CARTESIAN_POINT('Origin',(0.,0.,2.75));
#13283=CARTESIAN_POINT('Origin',(0.,0.,1.));
#13284=CARTESIAN_POINT('',(0.,0.,0.));
#13285=CARTESIAN_POINT('Origin',(-3.4,4.163799117101E-16,4.5));
#13286=CARTESIAN_POINT('',(-3.625,3.88825358729285E-16,4.6));
#13287=CARTESIAN_POINT('Origin',(-3.4,4.163799117101E-16,4.6));
#13288=CARTESIAN_POINT('',(-3.625,4.43934464690916E-16,5.));
#13289=CARTESIAN_POINT('',(-3.625,3.88825358729285E-16,4.5));
#13290=CARTESIAN_POINT('Origin',(-3.4,4.163799117101E-16,5.));
#13291=CARTESIAN_POINT('Origin',(2.0818995585505E-16,3.4,4.5));
#13292=CARTESIAN_POINT('',(-0.225,3.4,4.6));
#13293=CARTESIAN_POINT('Origin',(2.0818995585505E-16,3.4,4.6));
#13294=CARTESIAN_POINT('',(-0.225,3.4,5.));
#13295=CARTESIAN_POINT('',(-0.225,3.4,4.5));
#13296=CARTESIAN_POINT('Origin',(2.0818995585505E-16,3.4,5.));
#13297=CARTESIAN_POINT('Origin',(3.4,0.,4.5));
#13298=CARTESIAN_POINT('',(3.175,-2.75545529808155E-17,4.6));
#13299=CARTESIAN_POINT('Origin',(3.4,0.,4.6));
#13300=CARTESIAN_POINT('',(3.175,2.75545529808155E-17,5.));
#13301=CARTESIAN_POINT('',(3.175,-2.75545529808155E-17,4.5));
#13302=CARTESIAN_POINT('Origin',(3.4,0.,5.));
#13303=CARTESIAN_POINT('Origin',(-6.2456986756515E-16,-3.4,4.5));
#13304=CARTESIAN_POINT('',(-0.225000000000001,-3.4,4.6));
#13305=CARTESIAN_POINT('Origin',(-6.2456986756515E-16,-3.4,4.6));
#13306=CARTESIAN_POINT('',(-0.225000000000001,-3.4,5.));
#13307=CARTESIAN_POINT('',(-0.225000000000001,-3.4,4.5));
#13308=CARTESIAN_POINT('Origin',(-6.2456986756515E-16,-3.4,5.));
#13309=CARTESIAN_POINT('Origin',(0.,0.,4.25));
#13310=CARTESIAN_POINT('',(-2.59,-3.17183520979164E-16,4.6));
#13311=CARTESIAN_POINT('Origin',(0.,0.,4.6));
#13312=CARTESIAN_POINT('',(-2.59,-3.17183520979164E-16,4.25));
#13313=CARTESIAN_POINT('',(-2.59,-3.17183520979164E-16,4.25));
#13314=CARTESIAN_POINT('Origin',(0.,0.,4.25));
#13315=CARTESIAN_POINT('Origin',(0.,0.,4.25));
#13316=CARTESIAN_POINT('',(-2.,-2.44929359829471E-16,4.25));
#13317=CARTESIAN_POINT('Origin',(0.,0.,4.25));
#13318=CARTESIAN_POINT('Origin',(0.,0.,4.6));
#13319=CARTESIAN_POINT('',(-2.,-2.44929359829471E-16,5.));
#13320=CARTESIAN_POINT('Origin',(0.,0.,5.));
#13321=CARTESIAN_POINT('',(-2.,-2.44929359829471E-16,4.6));
#13322=CARTESIAN_POINT('Origin',(0.,0.,4.6));
#13323=CARTESIAN_POINT('',(-4.,-4.89858719658941E-16,5.));
#13324=CARTESIAN_POINT('Origin',(0.,0.,5.));
#13325=CARTESIAN_POINT('',(-4.,-4.89858719658941E-16,4.6));
#13326=CARTESIAN_POINT('',(-4.,-4.89858719658941E-16,4.6));
#13327=CARTESIAN_POINT('Origin',(0.,0.,4.6));
#13328=CARTESIAN_POINT('Origin',(0.,0.,5.));
#13329=CARTESIAN_POINT('Origin',(0.,0.,4.6));
#13330=CARTESIAN_POINT('',(0.,0.,0.));
#13331=CARTESIAN_POINT('Origin',(0.144337567297406,-0.6,-0.25));
#13332=CARTESIAN_POINT('',(0.288675134594813,-0.6,0.));
#13333=CARTESIAN_POINT('',(0.144337567297406,-0.6,-0.25));
#13334=CARTESIAN_POINT('',(0.288675134594813,-0.6,0.));
#13335=CARTESIAN_POINT('',(0.144337567297406,-0.96,-0.25));
#13336=CARTESIAN_POINT('',(0.144337567297406,-0.6,-0.25));
#13337=CARTESIAN_POINT('',(0.288675134594813,-0.96,0.));
#13338=CARTESIAN_POINT('',(0.288675134594813,-0.96,0.));
#13339=CARTESIAN_POINT('',(0.288675134594813,-0.6,0.));
#13340=CARTESIAN_POINT('Origin',(-0.144337567297406,-0.6,-0.25));
#13341=CARTESIAN_POINT('',(-0.144337567297406,-0.6,-0.25));
#13342=CARTESIAN_POINT('',(0.144337567297406,-0.6,-0.25));
#13343=CARTESIAN_POINT('',(-0.144337567297406,-0.96,-0.25));
#13344=CARTESIAN_POINT('',(-0.144337567297406,-0.6,-0.25));
#13345=CARTESIAN_POINT('',(0.144337567297406,-0.96,-0.25));
#13346=CARTESIAN_POINT('Origin',(-0.288675134594813,-0.6,-8.32667268468867E-17));
#13347=CARTESIAN_POINT('',(-0.288675134594813,-0.6,-3.53525079574969E-17));
#13348=CARTESIAN_POINT('',(-0.144337567297406,-0.6,-0.25));
#13349=CARTESIAN_POINT('',(-0.288675134594813,-0.96,-5.55111512312578E-17));
#13350=CARTESIAN_POINT('',(-0.288675134594813,-0.6,-3.53525079574969E-17));
#13351=CARTESIAN_POINT('',(-0.144337567297406,-0.96,-0.25));
#13352=CARTESIAN_POINT('Origin',(-0.144337567297407,-0.6,0.25));
#13353=CARTESIAN_POINT('',(-0.144337567297407,-0.6,0.25));
#13354=CARTESIAN_POINT('',(-0.288675134594813,-0.6,-3.53525079574969E-17));
#13355=CARTESIAN_POINT('',(-0.144337567297407,-0.96,0.25));
#13356=CARTESIAN_POINT('',(-0.144337567297407,-0.6,0.25));
#13357=CARTESIAN_POINT('',(-0.288675134594813,-0.96,-3.53525079574969E-17));
#13358=CARTESIAN_POINT('Origin',(0.144337567297406,-0.6,0.25));
#13359=CARTESIAN_POINT('',(0.144337567297406,-0.6,0.25));
#13360=CARTESIAN_POINT('',(-0.144337567297407,-0.6,0.25));
#13361=CARTESIAN_POINT('',(0.144337567297406,-0.96,0.25));
#13362=CARTESIAN_POINT('',(0.144337567297406,-0.6,0.25));
#13363=CARTESIAN_POINT('',(-0.144337567297407,-0.96,0.25));
#13364=CARTESIAN_POINT('Origin',(0.288675134594813,-0.6,0.));
#13365=CARTESIAN_POINT('',(0.144337567297406,-0.6,0.25));
#13366=CARTESIAN_POINT('',(0.144337567297406,-0.96,0.25));
#13367=CARTESIAN_POINT('Origin',(0.,-0.6,0.));
#13368=CARTESIAN_POINT('Origin',(0.,-0.96,0.));
#13369=CARTESIAN_POINT('Origin',(0.,-1.8,0.));
#13370=CARTESIAN_POINT('',(-0.2942,-1.8,3.60291088309151E-17));
#13371=CARTESIAN_POINT('Origin',(0.,-1.8,0.));
#13372=CARTESIAN_POINT('Origin',(0.45,0.6,0.));
#13373=CARTESIAN_POINT('',(-0.45,0.6,-5.51091059616309E-17));
#13374=CARTESIAN_POINT('Origin',(0.,0.6,0.));
#13375=CARTESIAN_POINT('Origin',(0.,0.575,0.));
#13376=CARTESIAN_POINT('',(-0.5,0.55,-6.12323399573677E-17));
#13377=CARTESIAN_POINT('Origin',(0.,0.55,0.));
#13378=CARTESIAN_POINT('',(-0.475,0.575,-5.81707229594993E-17));
#13379=CARTESIAN_POINT('Origin',(0.,0.29,0.));
#13380=CARTESIAN_POINT('',(-0.5,0.0299999999999998,-6.12323399573677E-17));
#13381=CARTESIAN_POINT('Origin',(0.,0.0299999999999998,0.));
#13382=CARTESIAN_POINT('',(-0.5,0.29,-6.12323399573677E-17));
#13383=CARTESIAN_POINT('Origin',(0.,0.0150000000000001,0.));
#13384=CARTESIAN_POINT('',(-0.47,7.11236625150491E-17,-5.75583995599256E-17));
#13385=CARTESIAN_POINT('Origin',(0.,0.,0.));
#13386=CARTESIAN_POINT('',(-0.485,0.0150000000000001,-5.93953697586466E-17));
#13387=CARTESIAN_POINT('Origin',(0.32,0.,0.));
#13388=CARTESIAN_POINT('',(-0.32,-6.93889390390723E-18,-3.91886975727153E-17));
#13389=CARTESIAN_POINT('Origin',(0.,0.,0.));
#13390=CARTESIAN_POINT('Origin',(0.,-0.02,0.));
#13391=CARTESIAN_POINT('',(-0.2942,-0.0515999999999999,3.60291088309151E-17));
#13392=CARTESIAN_POINT('Origin',(0.,-0.0515999999999999,0.));
#13393=CARTESIAN_POINT('',(-0.31,-0.02,-3.7964050773568E-17));
#13394=CARTESIAN_POINT('Origin',(0.,-1.24,0.));
#13395=CARTESIAN_POINT('',(-0.2942,-1.24,-3.60291088309151E-17));
#13396=CARTESIAN_POINT('',(0.,0.,0.));
#13397=CARTESIAN_POINT('',(0.,0.,0.));
#13398=CARTESIAN_POINT('Origin',(0.,0.,0.));
#13399=CARTESIAN_POINT('',(-1.88531,-0.410863395882378,-2.3088388569005E-16));
#13400=CARTESIAN_POINT('',(-2.3088388569005E-16,-0.410863395882378,1.88531));
#13401=CARTESIAN_POINT('Origin',(0.,-0.410863395882378,0.));
#13402=CARTESIAN_POINT('Origin',(0.,-0.410863395882378,0.));
#13403=CARTESIAN_POINT('',(-2.3088388569005E-16,0.410863395882378,1.88531));
#13404=CARTESIAN_POINT('Origin',(-2.35744508835865E-16,0.,1.925));
#13405=CARTESIAN_POINT('',(-1.88531,0.410863395882378,2.3088388569005E-16));
#13406=CARTESIAN_POINT('Origin',(0.,0.410863395882378,0.));
#13407=CARTESIAN_POINT('Origin',(0.,0.410863395882378,0.));
#13408=CARTESIAN_POINT('Origin',(0.,0.,0.));
#13409=CARTESIAN_POINT('',(-1.88531,0.75,-2.3088388569005E-16));
#13410=CARTESIAN_POINT('',(-1.88531,0.,-2.3088388569005E-16));
#13411=CARTESIAN_POINT('Origin',(0.,0.75,0.));
#13412=CARTESIAN_POINT('Origin',(0.,0.,0.));
#13413=CARTESIAN_POINT('',(-1.25,-0.65,-1.53080849893419E-16));
#13414=CARTESIAN_POINT('Origin',(0.,-0.65,0.));
#13415=CARTESIAN_POINT('',(-1.25,0.65,-1.53080849893419E-16));
#13416=CARTESIAN_POINT('',(-1.25,0.,-1.53080849893419E-16));
#13417=CARTESIAN_POINT('Origin',(0.,0.65,0.));
#13418=CARTESIAN_POINT('Origin',(0.,0.7,0.));
#13419=CARTESIAN_POINT('',(-1.35,0.75,-1.65327317884893E-16));
#13420=CARTESIAN_POINT('',(-1.3,0.7,-1.59204083889156E-16));
#13421=CARTESIAN_POINT('Origin',(0.,0.75,0.));
#13422=CARTESIAN_POINT('Origin',(1.88531,0.75,0.));
#13423=CARTESIAN_POINT('Origin',(0.,0.,0.));
#13424=CARTESIAN_POINT('',(-1.88531,-0.75,-2.3088388569005E-16));
#13425=CARTESIAN_POINT('Origin',(0.,-0.75,0.));
#13426=CARTESIAN_POINT('',(-1.88531,0.,-2.3088388569005E-16));
#13427=CARTESIAN_POINT('Origin',(1.35,-0.75,0.));
#13428=CARTESIAN_POINT('',(-1.35,-0.75,-1.65327317884893E-16));
#13429=CARTESIAN_POINT('Origin',(0.,-0.75,0.));
#13430=CARTESIAN_POINT('Origin',(0.,-0.7,0.));
#13431=CARTESIAN_POINT('',(-1.3,-0.7,-1.59204083889156E-16));
#13432=CARTESIAN_POINT('',(0.,0.,0.));
#13433=CARTESIAN_POINT('Origin',(0.,0.,0.));
#13434=CARTESIAN_POINT('',(-1.96469,0.410863395882378,-2.40605131981681E-16));
#13435=CARTESIAN_POINT('',(-2.40605131981681E-16,0.410863395882378,1.96469));
#13436=CARTESIAN_POINT('Origin',(0.,0.410863395882378,0.));
#13437=CARTESIAN_POINT('Origin',(0.,0.410863395882378,0.));
#13438=CARTESIAN_POINT('',(-2.40605131981681E-16,-0.410863395882378,1.96469));
#13439=CARTESIAN_POINT('Origin',(-2.35744508835865E-16,0.,1.925));
#13440=CARTESIAN_POINT('',(-1.96469,-0.410863395882378,2.40605131981681E-16));
#13441=CARTESIAN_POINT('Origin',(0.,-0.410863395882378,0.));
#13442=CARTESIAN_POINT('Origin',(0.,-0.410863395882378,0.));
#13443=CARTESIAN_POINT('Origin',(0.,0.,0.));
#13444=CARTESIAN_POINT('',(-1.96469,-0.75,-2.40605131981681E-16));
#13445=CARTESIAN_POINT('Origin',(0.,-0.75,0.));
#13446=CARTESIAN_POINT('',(-1.96469,0.,-2.40605131981681E-16));
#13447=CARTESIAN_POINT('Origin',(2.5,0.75,0.));
#13448=CARTESIAN_POINT('',(-2.5,0.75,-3.06161699786838E-16));
#13449=CARTESIAN_POINT('Origin',(0.,0.75,0.));
#13450=CARTESIAN_POINT('',(-1.96469,0.75,-2.40605131981681E-16));
#13451=CARTESIAN_POINT('Origin',(0.,0.75,0.));
#13452=CARTESIAN_POINT('Origin',(0.,0.7,0.));
#13453=CARTESIAN_POINT('',(-2.6,0.65,-3.18408167778312E-16));
#13454=CARTESIAN_POINT('Origin',(0.,0.65,0.));
#13455=CARTESIAN_POINT('',(-2.55,0.7,-3.12284933782575E-16));
#13456=CARTESIAN_POINT('Origin',(0.,0.,0.));
#13457=CARTESIAN_POINT('',(-2.6,-0.65,-3.18408167778312E-16));
#13458=CARTESIAN_POINT('Origin',(0.,-0.65,0.));
#13459=CARTESIAN_POINT('',(-2.6,0.,-3.18408167778312E-16));
#13460=CARTESIAN_POINT('Origin',(0.,-0.7,0.));
#13461=CARTESIAN_POINT('',(-2.5,-0.75,-3.06161699786838E-16));
#13462=CARTESIAN_POINT('Origin',(0.,-0.75,0.));
#13463=CARTESIAN_POINT('',(-2.55,-0.7,-3.12284933782575E-16));
#13464=CARTESIAN_POINT('Origin',(1.96469,-0.75,0.));
#13465=CARTESIAN_POINT('Origin',(0.,0.,0.));
#13466=CARTESIAN_POINT('',(-1.96469,0.,-2.40605131981681E-16));
#13467=CARTESIAN_POINT('',(0.,0.,0.));
#13468=CARTESIAN_POINT('Origin',(1.925,0.,0.));
#13469=CARTESIAN_POINT('',(1.925,-2.97627328869245E-33,0.3969));
#13470=CARTESIAN_POINT('',(1.925,-2.97627328869245E-33,-0.3969));
#13471=CARTESIAN_POINT('Origin',(1.925,0.,0.));
#13472=CARTESIAN_POINT('Origin',(1.47463555300403,0.,-1.23736614864659));
#13473=CARTESIAN_POINT('',(1.72975795528862,-2.97627328869245E-33,-0.933323109172666));
#13474=CARTESIAN_POINT('',(1.21951315071945,-2.97627328869245E-33,-1.54140918812051));
#13475=CARTESIAN_POINT('Origin',(1.47463555300403,0.,-1.23736614864659));
#13476=CARTESIAN_POINT('Origin',(0.334272742008841,0.,-1.8957549245485));
#13477=CARTESIAN_POINT('',(0.725142939179386,1.05214622327121E-34,-1.8268339628325));
#13478=CARTESIAN_POINT('',(-0.0565974551617042,-6.05776119971203E-33,-1.96467588626451));
#13479=CARTESIAN_POINT('Origin',(0.334272742008841,0.,-1.8957549245485));
#13480=CARTESIAN_POINT('Origin',(-0.9625,0.,-1.66709890228504));
#13481=CARTESIAN_POINT('',(-0.618774517237956,-2.97627328869245E-33,-1.86554890228504));
#13482=CARTESIAN_POINT('',(-1.30622548276204,-2.97627328869245E-33,-1.46864890228504));
#13483=CARTESIAN_POINT('Origin',(-0.9625,0.,-1.66709890228504));
#13484=CARTESIAN_POINT('Origin',(-1.80890829501287,0.,-0.658388775901913));
#13485=CARTESIAN_POINT('',(-1.67316050012692,1.05214622327121E-34,-1.03135277709184));
#13486=CARTESIAN_POINT('',(-1.94465608989883,-6.05776119971203E-33,-0.285424774711986));
#13487=CARTESIAN_POINT('Origin',(-1.80890829501287,0.,-0.658388775901913));
#13488=CARTESIAN_POINT('Origin',(-1.80890829501287,0.,0.658388775901912));
#13489=CARTESIAN_POINT('',(-1.94465608989883,-9.13924911073161E-33,0.285424774711985));
#13490=CARTESIAN_POINT('',(-1.67316050012692,3.1867025333467E-33,1.03135277709184));
#13491=CARTESIAN_POINT('Origin',(-1.80890829501287,0.,0.658388775901912));
#13492=CARTESIAN_POINT('Origin',(-0.962500000000001,0.,1.66709890228504));
#13493=CARTESIAN_POINT('',(-1.30622548276204,-2.97627328869245E-33,1.46864890228504));
#13494=CARTESIAN_POINT('',(-0.618774517237957,-2.97627328869245E-33,1.86554890228504));
#13495=CARTESIAN_POINT('Origin',(-0.962500000000001,0.,1.66709890228504));
#13496=CARTESIAN_POINT('Origin',(0.33427274200884,0.,1.8957549245485));
#13497=CARTESIAN_POINT('',(-0.0565974551617051,-2.97627328869245E-33,1.96467588626451));
#13498=CARTESIAN_POINT('',(0.725142939179386,-2.97627328869245E-33,1.8268339628325));
#13499=CARTESIAN_POINT('Origin',(0.33427274200884,0.,1.8957549245485));
#13500=CARTESIAN_POINT('Origin',(1.47463555300403,0.,1.23736614864659));
#13501=CARTESIAN_POINT('',(1.21951315071944,-6.05776119971203E-33,1.54140918812051));
#13502=CARTESIAN_POINT('',(1.72975795528862,1.05214622327122E-34,0.933323109172667));
#13503=CARTESIAN_POINT('Origin',(1.47463555300403,0.,1.23736614864659));
#13504=CARTESIAN_POINT('',(0.,0.,0.));
#13505=CARTESIAN_POINT('Origin',(1.47463555300403,0.,1.23736614864659));
#13506=CARTESIAN_POINT('',(1.16188454446795,-0.07938,1.49479506783723));
#13507=CARTESIAN_POINT('',(1.67384490577674,-0.07938,0.884664467981643));
#13508=CARTESIAN_POINT('Ctrl Pts',(1.16188454446795,-0.07938,1.49479506783723));
#13509=CARTESIAN_POINT('Ctrl Pts',(1.16869700612251,-0.123392992551698,
1.48949983100074));
#13510=CARTESIAN_POINT('Ctrl Pts',(1.18135446441955,-0.166529565724166,
1.47962830891229));
#13511=CARTESIAN_POINT('Ctrl Pts',(1.21282145231718,-0.237213819614884,
1.45388393800011));
#13512=CARTESIAN_POINT('Ctrl Pts',(1.22989120215288,-0.266247928944116,
1.4395843844684));
#13513=CARTESIAN_POINT('Ctrl Pts',(1.26813946847809,-0.317173992396757,
1.40600777299249));
#13514=CARTESIAN_POINT('Ctrl Pts',(1.28931069477441,-0.339063173951852,
1.38671820696899));
#13515=CARTESIAN_POINT('Ctrl Pts',(1.33224261954459,-0.373566122196588,
1.34549913552853));
#13516=CARTESIAN_POINT('Ctrl Pts',(1.35618281536764,-0.388075792674378,
1.32151296077672));
#13517=CARTESIAN_POINT('Ctrl Pts',(1.40439359896051,-0.407069005705619,
1.27016020894803));
#13518=CARTESIAN_POINT('Ctrl Pts',(1.42864614483643,-0.411552957311693,
1.24277684810113));
#13519=CARTESIAN_POINT('Ctrl Pts',(1.4719780748558,-0.411552957311693,1.19113586482651));
#13520=CARTESIAN_POINT('Ctrl Pts',(1.49473401052622,-0.407069005705619,
1.16249669890816));
#13521=CARTESIAN_POINT('Ctrl Pts',(1.53693488395083,-0.388075792674377,
1.10610103367387));
#13522=CARTESIAN_POINT('Ctrl Pts',(1.55639948343386,-0.373566122196588,
1.07835938768384));
#13523=CARTESIAN_POINT('Ctrl Pts',(1.58953729406031,-0.339063173951852,
1.02892207867768));
#13524=CARTESIAN_POINT('Ctrl Pts',(1.60485746336717,-0.317173992396757,
1.00472289289232));
#13525=CARTESIAN_POINT('Ctrl Pts',(1.63128222892223,-0.266247928944116,
0.961225186280959));
#13526=CARTESIAN_POINT('Ctrl Pts',(1.64240040915267,-0.237213819614884,
0.941931672888549));
#13527=CARTESIAN_POINT('Ctrl Pts',(1.66228948011831,-0.166529565724165,
0.906472276148935));
#13528=CARTESIAN_POINT('Ctrl Pts',(1.66981308703787,-0.123392992551698,
0.892292941263125));
#13529=CARTESIAN_POINT('Ctrl Pts',(1.67384490577674,-0.07938,0.884664467981643));
#13530=CARTESIAN_POINT('',(1.20622598189858,-0.07938,1.54074568637942));
#13531=CARTESIAN_POINT('Origin',(1.47463555300403,-0.07938,1.23736614864659));
#13532=CARTESIAN_POINT('',(1.72679724097776,-0.07938,0.920353018170519));
#13533=CARTESIAN_POINT('Ctrl Pts',(1.72679724097776,-0.0793800000000002,
0.920353018170518));
#13534=CARTESIAN_POINT('Ctrl Pts',(1.72470909046691,-0.10165971810728,0.92427087628551));
#13535=CARTESIAN_POINT('Ctrl Pts',(1.72169532435455,-0.123845306465941,
0.929898398578877));
#13536=CARTESIAN_POINT('Ctrl Pts',(1.70911544962889,-0.192537547974292,
0.952957916220029));
#13537=CARTESIAN_POINT('Ctrl Pts',(1.69580594901181,-0.236239311587943,
0.976785804874841));
#13538=CARTESIAN_POINT('Ctrl Pts',(1.66527150643903,-0.303218781300911,
1.02787962443771));
#13539=CARTESIAN_POINT('Ctrl Pts',(1.64438322958071,-0.3351607303803,1.06123747122987));
#13540=CARTESIAN_POINT('Ctrl Pts',(1.60730731395783,-0.3732673312795,1.11639170354769));
#13541=CARTESIAN_POINT('Ctrl Pts',(1.5873911192195,-0.387903357081022,1.1447096804553));
#13542=CARTESIAN_POINT('Ctrl Pts',(1.54427174765086,-0.40704475551587,1.20224605970712));
#13543=CARTESIAN_POINT('Ctrl Pts',(1.52104964294098,-0.411552957311693,
1.23144933316771));
#13544=CARTESIAN_POINT('Ctrl Pts',(1.47686834938291,-0.411552957311693,
1.284102548491));
#13545=CARTESIAN_POINT('Ctrl Pts',(1.45214121543005,-0.40704475551587,1.31204295246889));
#13546=CARTESIAN_POINT('Ctrl Pts',(1.40296654335764,-0.387903357081022,
1.36449833130133));
#13547=CARTESIAN_POINT('Ctrl Pts',(1.37853719107178,-0.3732673312795,1.38902931937536));
#13548=CARTESIAN_POINT('Ctrl Pts',(1.330659040657,-0.3351607303803,1.43511940046341));
#13549=CARTESIAN_POINT('Ctrl Pts',(1.30143518572334,-0.303218781300911,
1.4614828667669));
#13550=CARTESIAN_POINT('Ctrl Pts',(1.25641984639565,-0.236239311587943,
1.50042577120361));
#13551=CARTESIAN_POINT('Ctrl Pts',(1.23526512743829,-0.192537547974292,
1.51767074004259));
#13552=CARTESIAN_POINT('Ctrl Pts',(1.21474040800595,-0.123845306465941,
1.53406374142061));
#13553=CARTESIAN_POINT('Ctrl Pts',(1.20972171541452,-0.10165971810728,1.53800893064485));
#13554=CARTESIAN_POINT('Ctrl Pts',(1.20622598189858,-0.0793800000000002,
1.54074568637942));
#13555=CARTESIAN_POINT('Origin',(1.47463555300403,-0.07938,1.23736614864659));
#13556=CARTESIAN_POINT('Origin',(0.,-0.27783,0.));
#13557=CARTESIAN_POINT('',(0.731211914226578,-0.07938,1.81499518621871));
#13558=CARTESIAN_POINT('Origin',(0.,-0.07938,0.));
#13559=CARTESIAN_POINT('',(-0.0663495263035324,-0.07938,1.95562678695688));
#13560=CARTESIAN_POINT('Ctrl Pts',(0.73121191422658,-0.0793800000000002,
1.81499518621871));
#13561=CARTESIAN_POINT('Ctrl Pts',(0.727093947478514,-0.10165971810728,
1.81665420238109));
#13562=CARTESIAN_POINT('Ctrl Pts',(0.721167967091869,-0.123845306465941,
1.81902792304693));
#13563=CARTESIAN_POINT('Ctrl Pts',(0.696708851738065,-0.192537547974292,
1.82860635079188));
#13564=CARTESIAN_POINT('Ctrl Pts',(0.671196911157359,-0.236239311587943,
1.83830439039938));
#13565=CARTESIAN_POINT('Ctrl Pts',(0.614963696954177,-0.303218781300911,
1.85781736559878));
#13566=CARTESIAN_POINT('Ctrl Pts',(0.577520337936704,-0.3351607303803,1.86994423321609));
#13567=CARTESIAN_POINT('Ctrl Pts',(0.513666081644577,-0.3732673312795,1.88836288721748));
#13568=CARTESIAN_POINT('Ctrl Pts',(0.48020694664961,-0.387903357081022,
1.89725383285802));
#13569=CARTESIAN_POINT('Ctrl Pts',(0.410191919979371,-0.40704475551587,
1.91361265867928));
#13570=CARTESIAN_POINT('Ctrl Pts',(0.373631253366087,-0.411552957311693,
1.92105678285629));
#13571=CARTESIAN_POINT('Ctrl Pts',(0.305941584526154,-0.411552957311693,
1.932992297788));
#13572=CARTESIAN_POINT('Ctrl Pts',(0.269039755480681,-0.40704475551587,
1.9385015936658));
#13573=CARTESIAN_POINT('Ctrl Pts',(0.197652103622503,-0.387903357081022,
1.94707587521355));
#13574=CARTESIAN_POINT('Ctrl Pts',(0.163169918867575,-0.3732673312795,1.95016481734985));
#13575=CARTESIAN_POINT('Ctrl Pts',(0.09686699474267,-0.3351607303803,1.95469638598893));
#13576=CARTESIAN_POINT('Ctrl Pts',(0.0575341135759475,-0.30321878130091,
1.95610724099344));
#13577=CARTESIAN_POINT('Ctrl Pts',(-0.00198165342826295,-0.236239311587942,
1.95700393417042));
#13578=CARTESIAN_POINT('Ctrl Pts',(-0.0292719606304177,-0.192537547974292,
1.95661635548909));
#13579=CARTESIAN_POINT('Ctrl Pts',(-0.0555320260694991,-0.123845306465941,
1.95598108775736));
#13580=CARTESIAN_POINT('Ctrl Pts',(-0.0619124863920986,-0.10165971810728,
1.95577732462505));
#13581=CARTESIAN_POINT('Ctrl Pts',(-0.0663495263035336,-0.0793800000000002,
1.95562678695688));
#13582=CARTESIAN_POINT('',(-0.606515593706441,-0.07938,1.86038093521056));
#13583=CARTESIAN_POINT('Origin',(0.,-0.07938,0.));
#13584=CARTESIAN_POINT('',(-1.30787935375538,-0.07938,1.45544837954646));
#13585=CARTESIAN_POINT('Ctrl Pts',(-0.60651559370644,-0.0793800000000002,
1.86038093521056));
#13586=CARTESIAN_POINT('Ctrl Pts',(-0.610736534284191,-0.10165971810728,
1.85900483732004));
#13587=CARTESIAN_POINT('Ctrl Pts',(-0.616801896862274,-0.123845306465941,
1.85701406607784));
#13588=CARTESIAN_POINT('Ctrl Pts',(-0.64169556093739,-0.192537547974292,
1.84862955113236));
#13589=CARTESIAN_POINT('Ctrl Pts',(-0.667472620950374,-0.236239311587943,
1.8396599211785));
#13590=CARTESIAN_POINT('Ctrl Pts',(-0.723092460895733,-0.303218781300911,
1.81846171405606));
#13591=CARTESIAN_POINT('Ctrl Pts',(-0.759570738251496,-0.3351607303803,
1.80368330636526));
#13592=CARTESIAN_POINT('Ctrl Pts',(-0.820325219032771,-0.3732673312795,
1.77674808914243));
#13593=CARTESIAN_POINT('Ctrl Pts',(-0.851671393163369,-0.387903357081022,
1.76205183123884));
#13594=CARTESIAN_POINT('Ctrl Pts',(-0.915821265825857,-0.40704475551587,
1.72957862721967));
#13595=CARTESIAN_POINT('Ctrl Pts',(-0.948613352107641,-0.411552957311693,
1.71178041367846));
#13596=CARTESIAN_POINT('Ctrl Pts',(-1.00813864789236,-0.411552957311693,
1.67741346813356));
#13597=CARTESIAN_POINT('Ctrl Pts',(-1.03994839610192,-0.40704475551587,
1.65791379514105));
#13598=CARTESIAN_POINT('Ctrl Pts',(-1.10014595205605,-0.387903357081022,
1.61859497777538));
#13599=CARTESIAN_POINT('Ctrl Pts',(-1.12854637180642,-0.3732673312795,1.59879652361863));
#13600=CARTESIAN_POINT('Ctrl Pts',(-1.18225019456848,-0.3351607303803,1.55964920847973));
#13601=CARTESIAN_POINT('Ctrl Pts',(-1.21328780973407,-0.30321878130091,
1.53544729744874));
#13602=CARTESIAN_POINT('Ctrl Pts',(-1.25945591558947,-0.236239311587942,
1.49787820666285));
#13603=CARTESIAN_POINT('Ctrl Pts',(-1.28011237299855,-0.192537547974292,
1.48003943283366));
#13604=CARTESIAN_POINT('Ctrl Pts',(-1.29982040797731,-0.12384530646594,
1.46267314482408));
#13605=CARTESIAN_POINT('Ctrl Pts',(-1.30457714773522,-0.10165971810728,
1.45841577236939));
#13606=CARTESIAN_POINT('Ctrl Pts',(-1.30787935375538,-0.0793800000000002,
1.45544837954646));
#13607=CARTESIAN_POINT('',(-1.66044771467423,-0.07938,1.03527376878636));
#13608=CARTESIAN_POINT('Origin',(0.,-0.07938,0.));
#13609=CARTESIAN_POINT('',(-1.93743789612516,-0.07938,0.274249499839291));
#13610=CARTESIAN_POINT('Ctrl Pts',(-1.66044771467423,-0.0793800000000002,
1.03527376878636));
#13611=CARTESIAN_POINT('Ctrl Pts',(-1.66279660407481,-0.10165971810728,
1.03150644833954));
#13612=CARTESIAN_POINT('Ctrl Pts',(-1.66616329828505,-0.123845306465941,
1.02608268917849));
#13613=CARTESIAN_POINT('Ctrl Pts',(-1.67984348899847,-0.192537547974292,
1.00365843926907));
#13614=CARTESIAN_POINT('Ctrl Pts',(-1.69382429558355,-0.236239311587943,
0.980218129295584));
#13615=CARTESIAN_POINT('Ctrl Pts',(-1.72280562001498,-0.303218781300911,
0.928227616555729));
#13616=CARTESIAN_POINT('Ctrl Pts',(-1.74125022432338,-0.3351607303803,0.893458914759057));
#13617=CARTESIAN_POINT('Ctrl Pts',(-1.7704772328254,-0.3732673312795,0.833773113802161));
#13618=CARTESIAN_POINT('Ctrl Pts',(-1.785043222842,-0.387903357081022,0.802366194758251));
#13619=CARTESIAN_POINT('Ctrl Pts',(-1.81331150313154,-0.407044755515871,
0.736255533958675));
#13620=CARTESIAN_POINT('Ctrl Pts',(-1.82699122746714,-0.411552957311693,
0.701542964620283));
#13621=CARTESIAN_POINT('Ctrl Pts',(-1.850499602749,-0.411552957311693,0.636954234365294));
#13622=CARTESIAN_POINT('Ctrl Pts',(-1.86233313540942,-0.40704475551587,
0.60156970621039));
#13623=CARTESIAN_POINT('Ctrl Pts',(-1.88317349000725,-0.387903357081022,
0.53275550155669));
#13624=CARTESIAN_POINT('Ctrl Pts',(-1.89220327271636,-0.3732673312795,0.499333567842125));
#13625=CARTESIAN_POINT('Ctrl Pts',(-1.9081793785937,-0.3351607303803,0.434824832752687));
#13626=CARTESIAN_POINT('Ctrl Pts',(-1.91639888267751,-0.30321878130091,
0.396334498831876));
#13627=CARTESIAN_POINT('Ctrl Pts',(-1.92761675755301,-0.236239311587942,
0.337878619195771));
#13628=CARTESIAN_POINT('Ctrl Pts',(-1.93197397917636,-0.192537547974292,
0.310935610749289));
#13629=CARTESIAN_POINT('Ctrl Pts',(-1.93590837509782,-0.12384530646594,
0.284964181626328));
#13630=CARTESIAN_POINT('Ctrl Pts',(-1.93681566289304,-0.10165971810728,
0.278645271736243));
#13631=CARTESIAN_POINT('Ctrl Pts',(-1.93743789612516,-0.0793800000000002,
0.27424949983929));
#13632=CARTESIAN_POINT('',(-1.956752,-0.07938,2.39633007352518E-16));
#13633=CARTESIAN_POINT('Origin',(0.,-0.07938,0.));
#13634=CARTESIAN_POINT('',(-1.956752,-0.47628,2.39633007352518E-16));
#13635=CARTESIAN_POINT('',(-1.956752,-0.27783,2.39633007352518E-16));
#13636=CARTESIAN_POINT('Origin',(0.,-0.47628,0.));
#13637=CARTESIAN_POINT('',(-1.93743789612516,-0.07938,-0.274249499839292));
#13638=CARTESIAN_POINT('Origin',(0.,-0.07938,0.));
#13639=CARTESIAN_POINT('',(-1.66044771467423,-0.07938,-1.03527376878636));
#13640=CARTESIAN_POINT('Ctrl Pts',(-1.93743789612516,-0.0793800000000002,
-0.27424949983929));
#13641=CARTESIAN_POINT('Ctrl Pts',(-1.93681566289304,-0.10165971810728,
-0.278645271736244));
#13642=CARTESIAN_POINT('Ctrl Pts',(-1.93590837509782,-0.123845306465941,
-0.284964181626328));
#13643=CARTESIAN_POINT('Ctrl Pts',(-1.93197397917636,-0.192537547974292,
-0.310935610749289));
#13644=CARTESIAN_POINT('Ctrl Pts',(-1.92761675755301,-0.236239311587942,
-0.337878619195772));
#13645=CARTESIAN_POINT('Ctrl Pts',(-1.91639888267751,-0.303218781300911,
-0.396334498831877));
#13646=CARTESIAN_POINT('Ctrl Pts',(-1.9081793785937,-0.3351607303803,-0.434824832752687));
#13647=CARTESIAN_POINT('Ctrl Pts',(-1.89220327271636,-0.3732673312795,-0.499333567842125));
#13648=CARTESIAN_POINT('Ctrl Pts',(-1.88317349000725,-0.387903357081022,
-0.53275550155669));
#13649=CARTESIAN_POINT('Ctrl Pts',(-1.86233313540942,-0.40704475551587,
-0.601569706210391));
#13650=CARTESIAN_POINT('Ctrl Pts',(-1.850499602749,-0.411552957311693,-0.636954234365295));
#13651=CARTESIAN_POINT('Ctrl Pts',(-1.82699122746714,-0.411552957311693,
-0.701542964620284));
#13652=CARTESIAN_POINT('Ctrl Pts',(-1.81331150313154,-0.40704475551587,
-0.736255533958675));
#13653=CARTESIAN_POINT('Ctrl Pts',(-1.785043222842,-0.387903357081022,-0.802366194758251));
#13654=CARTESIAN_POINT('Ctrl Pts',(-1.7704772328254,-0.3732673312795,-0.833773113802161));
#13655=CARTESIAN_POINT('Ctrl Pts',(-1.74125022432338,-0.3351607303803,-0.893458914759057));
#13656=CARTESIAN_POINT('Ctrl Pts',(-1.72280562001498,-0.303218781300911,
-0.92822761655573));
#13657=CARTESIAN_POINT('Ctrl Pts',(-1.69382429558355,-0.236239311587942,
-0.980218129295584));
#13658=CARTESIAN_POINT('Ctrl Pts',(-1.67984348899847,-0.192537547974292,
-1.00365843926907));
#13659=CARTESIAN_POINT('Ctrl Pts',(-1.66616329828505,-0.123845306465941,
-1.02608268917849));
#13660=CARTESIAN_POINT('Ctrl Pts',(-1.66279660407481,-0.10165971810728,
-1.03150644833954));
#13661=CARTESIAN_POINT('Ctrl Pts',(-1.66044771467423,-0.0793800000000001,
-1.03527376878636));
#13662=CARTESIAN_POINT('',(-1.30787935375538,-0.07938,-1.45544837954646));
#13663=CARTESIAN_POINT('Origin',(0.,-0.07938,0.));
#13664=CARTESIAN_POINT('',(-0.60651559370644,-0.07938,-1.86038093521056));
#13665=CARTESIAN_POINT('Ctrl Pts',(-1.30787935375538,-0.0793800000000002,
-1.45544837954646));
#13666=CARTESIAN_POINT('Ctrl Pts',(-1.30457714773522,-0.10165971810728,
-1.45841577236939));
#13667=CARTESIAN_POINT('Ctrl Pts',(-1.29982040797731,-0.123845306465941,
-1.46267314482408));
#13668=CARTESIAN_POINT('Ctrl Pts',(-1.28011237299855,-0.192537547974292,
-1.48003943283366));
#13669=CARTESIAN_POINT('Ctrl Pts',(-1.25945591558947,-0.236239311587942,
-1.49787820666285));
#13670=CARTESIAN_POINT('Ctrl Pts',(-1.21328780973407,-0.303218781300911,
-1.53544729744874));
#13671=CARTESIAN_POINT('Ctrl Pts',(-1.18225019456848,-0.3351607303803,-1.55964920847973));
#13672=CARTESIAN_POINT('Ctrl Pts',(-1.12854637180642,-0.3732673312795,-1.59879652361863));
#13673=CARTESIAN_POINT('Ctrl Pts',(-1.10014595205605,-0.387903357081022,
-1.61859497777538));
#13674=CARTESIAN_POINT('Ctrl Pts',(-1.03994839610192,-0.40704475551587,
-1.65791379514105));
#13675=CARTESIAN_POINT('Ctrl Pts',(-1.00813864789236,-0.411552957311693,
-1.67741346813356));
#13676=CARTESIAN_POINT('Ctrl Pts',(-0.948613352107639,-0.411552957311693,
-1.71178041367846));
#13677=CARTESIAN_POINT('Ctrl Pts',(-0.915821265825855,-0.40704475551587,
-1.72957862721967));
#13678=CARTESIAN_POINT('Ctrl Pts',(-0.851671393163367,-0.387903357081022,
-1.76205183123885));
#13679=CARTESIAN_POINT('Ctrl Pts',(-0.820325219032769,-0.3732673312795,
-1.77674808914243));
#13680=CARTESIAN_POINT('Ctrl Pts',(-0.759570738251494,-0.3351607303803,
-1.80368330636526));
#13681=CARTESIAN_POINT('Ctrl Pts',(-0.723092460895731,-0.303218781300911,
-1.81846171405606));
#13682=CARTESIAN_POINT('Ctrl Pts',(-0.667472620950373,-0.236239311587942,
-1.8396599211785));
#13683=CARTESIAN_POINT('Ctrl Pts',(-0.641695560937389,-0.192537547974292,
-1.84862955113236));
#13684=CARTESIAN_POINT('Ctrl Pts',(-0.616801896862272,-0.123845306465941,
-1.85701406607784));
#13685=CARTESIAN_POINT('Ctrl Pts',(-0.610736534284189,-0.10165971810728,
-1.85900483732004));
#13686=CARTESIAN_POINT('Ctrl Pts',(-0.606515593706439,-0.0793800000000002,
-1.86038093521056));
#13687=CARTESIAN_POINT('',(-0.0663495263035315,-0.07938,-1.95562678695688));
#13688=CARTESIAN_POINT('Origin',(0.,-0.07938,0.));
#13689=CARTESIAN_POINT('',(0.731211914226579,-0.07938,-1.81499518621871));
#13690=CARTESIAN_POINT('Ctrl Pts',(-0.0663495263035327,-0.0793800000000002,
-1.95562678695688));
#13691=CARTESIAN_POINT('Ctrl Pts',(-0.0619124863920977,-0.10165971810728,
-1.95577732462505));
#13692=CARTESIAN_POINT('Ctrl Pts',(-0.0555320260694982,-0.123845306465941,
-1.95598108775736));
#13693=CARTESIAN_POINT('Ctrl Pts',(-0.0292719606304167,-0.192537547974292,
-1.95661635548909));
#13694=CARTESIAN_POINT('Ctrl Pts',(-0.00198165342826177,-0.236239311587943,
-1.95700393417042));
#13695=CARTESIAN_POINT('Ctrl Pts',(0.0575341135759488,-0.303218781300911,
-1.95610724099344));
#13696=CARTESIAN_POINT('Ctrl Pts',(0.0968669947426714,-0.3351607303803,
-1.95469638598893));
#13697=CARTESIAN_POINT('Ctrl Pts',(0.163169918867576,-0.3732673312795,-1.95016481734985));
#13698=CARTESIAN_POINT('Ctrl Pts',(0.197652103622504,-0.387903357081022,
-1.94707587521355));
#13699=CARTESIAN_POINT('Ctrl Pts',(0.269039755480682,-0.40704475551587,
-1.9385015936658));
#13700=CARTESIAN_POINT('Ctrl Pts',(0.305941584526155,-0.411552957311693,
-1.93299229778799));
#13701=CARTESIAN_POINT('Ctrl Pts',(0.373631253366089,-0.411552957311693,
-1.92105678285629));
#13702=CARTESIAN_POINT('Ctrl Pts',(0.410191919979372,-0.40704475551587,
-1.91361265867928));
#13703=CARTESIAN_POINT('Ctrl Pts',(0.480206946649611,-0.387903357081022,
-1.89725383285802));
#13704=CARTESIAN_POINT('Ctrl Pts',(0.513666081644578,-0.3732673312795,-1.88836288721748));
#13705=CARTESIAN_POINT('Ctrl Pts',(0.577520337936705,-0.3351607303803,-1.86994423321609));
#13706=CARTESIAN_POINT('Ctrl Pts',(0.614963696954178,-0.30321878130091,
-1.85781736559878));
#13707=CARTESIAN_POINT('Ctrl Pts',(0.67119691115736,-0.236239311587942,
-1.83830439039938));
#13708=CARTESIAN_POINT('Ctrl Pts',(0.696708851738067,-0.192537547974292,
-1.82860635079188));
#13709=CARTESIAN_POINT('Ctrl Pts',(0.721167967091869,-0.123845306465941,
-1.81902792304693));
#13710=CARTESIAN_POINT('Ctrl Pts',(0.727093947478515,-0.10165971810728,
-1.81665420238109));
#13711=CARTESIAN_POINT('Ctrl Pts',(0.73121191422658,-0.0793800000000002,
-1.81499518621871));
#13712=CARTESIAN_POINT('',(1.20622598189858,-0.07938,-1.54074568637942));
#13713=CARTESIAN_POINT('Origin',(0.,-0.07938,0.));
#13714=CARTESIAN_POINT('',(1.72679724097776,-0.07938,-0.920353018170518));
#13715=CARTESIAN_POINT('Ctrl Pts',(1.20622598189858,-0.0793800000000002,
-1.54074568637942));
#13716=CARTESIAN_POINT('Ctrl Pts',(1.20972171541452,-0.10165971810728,-1.53800893064485));
#13717=CARTESIAN_POINT('Ctrl Pts',(1.21474040800596,-0.123845306465941,
-1.53406374142061));
#13718=CARTESIAN_POINT('Ctrl Pts',(1.23526512743829,-0.192537547974292,
-1.51767074004259));
#13719=CARTESIAN_POINT('Ctrl Pts',(1.25641984639565,-0.236239311587942,
-1.50042577120361));
#13720=CARTESIAN_POINT('Ctrl Pts',(1.30143518572334,-0.303218781300911,
-1.4614828667669));
#13721=CARTESIAN_POINT('Ctrl Pts',(1.330659040657,-0.3351607303803,-1.43511940046341));
#13722=CARTESIAN_POINT('Ctrl Pts',(1.37853719107178,-0.3732673312795,-1.38902931937536));
#13723=CARTESIAN_POINT('Ctrl Pts',(1.40296654335764,-0.387903357081022,
-1.36449833130133));
#13724=CARTESIAN_POINT('Ctrl Pts',(1.45214121543005,-0.40704475551587,-1.31204295246889));
#13725=CARTESIAN_POINT('Ctrl Pts',(1.47686834938291,-0.411552957311693,
-1.284102548491));
#13726=CARTESIAN_POINT('Ctrl Pts',(1.52104964294098,-0.411552957311693,
-1.23144933316771));
#13727=CARTESIAN_POINT('Ctrl Pts',(1.54427174765086,-0.407044755515871,
-1.20224605970712));
#13728=CARTESIAN_POINT('Ctrl Pts',(1.5873911192195,-0.387903357081022,-1.1447096804553));
#13729=CARTESIAN_POINT('Ctrl Pts',(1.60730731395783,-0.3732673312795,-1.11639170354769));
#13730=CARTESIAN_POINT('Ctrl Pts',(1.64438322958071,-0.3351607303803,-1.06123747122987));
#13731=CARTESIAN_POINT('Ctrl Pts',(1.66527150643903,-0.303218781300911,
-1.02787962443771));
#13732=CARTESIAN_POINT('Ctrl Pts',(1.69580594901181,-0.236239311587943,
-0.976785804874841));
#13733=CARTESIAN_POINT('Ctrl Pts',(1.70911544962889,-0.192537547974292,
-0.952957916220028));
#13734=CARTESIAN_POINT('Ctrl Pts',(1.72169532435455,-0.123845306465941,
-0.929898398578876));
#13735=CARTESIAN_POINT('Ctrl Pts',(1.72470909046691,-0.10165971810728,-0.924270876285509));
#13736=CARTESIAN_POINT('Ctrl Pts',(1.72679724097776,-0.0793800000000002,
-0.920353018170518));
#13737=CARTESIAN_POINT('',(1.91439494746182,-0.07938,-0.404932555664102));
#13738=CARTESIAN_POINT('Origin',(0.,-0.07938,0.));
#13739=CARTESIAN_POINT('',(1.91439494746182,-0.07938,0.404932555664102));
#13740=CARTESIAN_POINT('Ctrl Pts',(1.91439494746182,-0.0793800000000002,
-0.404932555664103));
#13741=CARTESIAN_POINT('Ctrl Pts',(1.91531368201941,-0.10165971810728,-0.400589064950645));
#13742=CARTESIAN_POINT('Ctrl Pts',(1.91662230483958,-0.123845306465941,
-0.394340921253764));
#13743=CARTESIAN_POINT('Ctrl Pts',(1.92180793393594,-0.192537547974292,
-0.368590118298695));
#13744=CARTESIAN_POINT('Ctrl Pts',(1.92692853653984,-0.236239311587943,
-0.341781714515643));
#13745=CARTESIAN_POINT('Ctrl Pts',(1.9363802706298,-0.303218781300911,-0.283014416607319));
#13746=CARTESIAN_POINT('Ctrl Pts',(1.94182093281998,-0.3351607303803,-0.244034097885537));
#13747=CARTESIAN_POINT('Ctrl Pts',(1.94887159083919,-0.3732673312795,-0.177951565523803));
#13748=CARTESIAN_POINT('Ctrl Pts',(1.95181734521941,-0.387903357081022,
-0.143456853463462));
#13749=CARTESIAN_POINT('Ctrl Pts',(1.95576966192778,-0.40704475551587,-0.071664832078622));
#13750=CARTESIAN_POINT('Ctrl Pts',(1.956752,-0.411552957311693,-0.0343669455449008));
#13751=CARTESIAN_POINT('Ctrl Pts',(1.956752,-0.411552957311693,0.0343669455449008));
#13752=CARTESIAN_POINT('Ctrl Pts',(1.95576966192778,-0.40704475551587,0.0716648320786219));
#13753=CARTESIAN_POINT('Ctrl Pts',(1.95181734521941,-0.387903357081022,
0.143456853463462));
#13754=CARTESIAN_POINT('Ctrl Pts',(1.94887159083919,-0.3732673312795,0.177951565523803));
#13755=CARTESIAN_POINT('Ctrl Pts',(1.94182093281998,-0.3351607303803,0.244034097885537));
#13756=CARTESIAN_POINT('Ctrl Pts',(1.9363802706298,-0.303218781300911,0.283014416607319));
#13757=CARTESIAN_POINT('Ctrl Pts',(1.92692853653984,-0.236239311587943,
0.341781714515643));
#13758=CARTESIAN_POINT('Ctrl Pts',(1.92180793393594,-0.192537547974292,
0.368590118298695));
#13759=CARTESIAN_POINT('Ctrl Pts',(1.91662230483958,-0.123845306465941,
0.394340921253764));
#13760=CARTESIAN_POINT('Ctrl Pts',(1.91531368201941,-0.10165971810728,0.400589064950645));
#13761=CARTESIAN_POINT('Ctrl Pts',(1.91439494746182,-0.0793800000000002,
0.404932555664103));
#13762=CARTESIAN_POINT('Origin',(0.,-0.07938,0.));
#13763=CARTESIAN_POINT('Origin',(0.,-0.07938,0.));
#13764=CARTESIAN_POINT('',(0.71358822996475,-0.07938,1.75361906569237));
#13765=CARTESIAN_POINT('Origin',(0.,-0.07938,0.));
#13766=CARTESIAN_POINT('Origin',(0.33427274200884,-0.07938,1.8957549245485));
#13767=CARTESIAN_POINT('Origin',(0.33427274200884,0.,1.8957549245485));
#13768=CARTESIAN_POINT('',(-0.070780549790825,-0.07938,1.89192444438865));
#13769=CARTESIAN_POINT('Ctrl Pts',(-0.0707805497908251,-0.07938,1.89192444438865));
#13770=CARTESIAN_POINT('Ctrl Pts',(-0.0621581887675352,-0.123392992551698,
1.89224702357808));
#13771=CARTESIAN_POINT('Ctrl Pts',(-0.0461167210878756,-0.166529565724166,
1.89282105630055));
#13772=CARTESIAN_POINT('Ctrl Pts',(-0.00546344722567869,-0.237213819614884,
1.89332631395644));
#13773=CARTESIAN_POINT('Ctrl Pts',(0.0168043156156246,-0.266247928944116,
1.89334444412923));
#13774=CARTESIAN_POINT('Ctrl Pts',(0.0676868173249578,-0.317173992396757,
1.89220877917518));
#13775=CARTESIAN_POINT('Ctrl Pts',(0.0963040116194015,-0.339063173951852,
1.89104071625784));
#13776=CARTESIAN_POINT('Ctrl Pts',(0.155686882426711,-0.373566122196588,
1.88706118493262));
#13777=CARTESIAN_POINT('Ctrl Pts',(0.189444152338378,-0.388075792674378,
1.88407517030084));
#13778=CARTESIAN_POINT('Ctrl Pts',(0.259384667806906,-0.407069005705619,
1.87572597447038));
#13779=CARTESIAN_POINT('Ctrl Pts',(0.295564880870602,-0.411552957311693,
1.87033833905209));
#13780=CARTESIAN_POINT('Ctrl Pts',(0.361953249272518,-0.411552957311693,
1.85863227849762));
#13781=CARTESIAN_POINT('Ctrl Pts',(0.397794208344885,-0.407069005705619,
1.85132063808607));
#13782=CARTESIAN_POINT('Ctrl Pts',(0.466372387779211,-0.388075792674377,
1.83524525067264));
#13783=CARTESIAN_POINT('Ctrl Pts',(0.499115122365417,-0.373566122196588,
1.82650552029421));
#13784=CARTESIAN_POINT('Ctrl Pts',(0.55627784773835,-0.339063173951852,
1.8099349185301));
#13785=CARTESIAN_POINT('Ctrl Pts',(0.583568715090836,-0.317173992396757,
1.80124488173997));
#13786=CARTESIAN_POINT('Ctrl Pts',(0.631771046764577,-0.266247928944116,
1.78490921718958));
#13787=CARTESIAN_POINT('Ctrl Pts',(0.652689698303665,-0.237213819614884,
1.77727615696148));
#13788=CARTESIAN_POINT('Ctrl Pts',(0.690718471466875,-0.166529565724165,
1.76289713151763));
#13789=CARTESIAN_POINT('Ctrl Pts',(0.705596189518013,-0.123392992551698,
1.75687121212928));
#13790=CARTESIAN_POINT('Ctrl Pts',(0.71358822996475,-0.07938,1.75361906569237));
#13791=CARTESIAN_POINT('Origin',(0.33427274200884,-0.07938,1.8957549245485));
#13792=CARTESIAN_POINT('Origin',(0.,-0.07938,0.));
#13793=CARTESIAN_POINT('',(-0.580564309297537,-0.07938,1.80203581326062));
#13794=CARTESIAN_POINT('Origin',(0.,-0.07938,0.));
#13795=CARTESIAN_POINT('Origin',(-0.962500000000001,-0.07938,1.66709890228504));
#13796=CARTESIAN_POINT('Origin',(-0.962500000000001,0.,1.66709890228504));
#13797=CARTESIAN_POINT('',(-1.27032663816428,-0.07938,1.40380134701254));
#13798=CARTESIAN_POINT('Ctrl Pts',(-1.27032663816428,-0.07938,1.40380134701254));
#13799=CARTESIAN_POINT('Ctrl Pts',(-1.26392887632193,-0.123392992551698,
1.40959080384008));
#13800=CARTESIAN_POINT('Ctrl Pts',(-1.25200938026802,-0.166529565724166,
1.42034179508297));
#13801=CARTESIAN_POINT('Ctrl Pts',(-1.22119193909219,-0.237213819614885,
1.44686026563443));
#13802=CARTESIAN_POINT('Ctrl Pts',(-1.20414549695735,-0.266247928944117,
1.46118759620237));
#13803=CARTESIAN_POINT('Ctrl Pts',(-1.16443724790971,-0.317173992396758,
1.49302426802369));
#13804=CARTESIAN_POINT('Ctrl Pts',(-1.14176438887219,-0.339063173951853,
1.51052425783311));
#13805=CARTESIAN_POINT('Ctrl Pts',(-1.09371647724559,-0.373566122196589,
1.54564633355776));
#13806=CARTESIAN_POINT('Ctrl Pts',(-1.06593753500724,-0.388075792674378,
1.56505766847808));
#13807=CARTESIAN_POINT('Ctrl Pts',(-1.00699323215303,-0.407069005705619,
1.6036187101659));
#13808=CARTESIAN_POINT('Ctrl Pts',(-0.975814475692339,-0.411552957311693,
1.62274773466534));
#13809=CARTESIAN_POINT('Ctrl Pts',(-0.917433524307661,-0.411552957311693,
1.65645399266283));
#13810=CARTESIAN_POINT('Ctrl Pts',(-0.885277924911194,-0.407069005705619,
1.67389107556648));
#13811=CARTESIAN_POINT('Ctrl Pts',(-0.822410931786043,-0.388075792674377,
1.70565781840267));
#13812=CARTESIAN_POINT('Ctrl Pts',(-0.791710751504505,-0.373566122196588,
1.72000942061118));
#13813=CARTESIAN_POINT('Ctrl Pts',(-0.737270185880016,-0.339063173951852,
1.74405909481629));
#13814=CARTESIAN_POINT('Ctrl Pts',(-0.710778320620332,-0.317173992396757,
1.75494437181449));
#13815=CARTESIAN_POINT('Ctrl Pts',(-0.663352829527299,-0.266247928944116,
1.77341438831889));
#13816=CARTESIAN_POINT('Ctrl Pts',(-0.642421776219621,-0.237213819614884,
1.78101337496783));
#13817=CARTESIAN_POINT('Ctrl Pts',(-0.604047386464641,-0.166529565724165,
1.79444282663));
#13818=CARTESIAN_POINT('Ctrl Pts',(-0.588777006905475,-0.123392992551698,
1.79938991739155));
#13819=CARTESIAN_POINT('Ctrl Pts',(-0.580564309297537,-0.0793799999999999,
1.80203581326062));
#13820=CARTESIAN_POINT('Origin',(-0.962500000000001,-0.07938,1.66709890228504));
#13821=CARTESIAN_POINT('Origin',(0.,-0.07938,0.));
#13822=CARTESIAN_POINT('',(-1.60306435598592,-0.07938,1.00725997640701));
#13823=CARTESIAN_POINT('Origin',(0.,-0.07938,0.));
#13824=CARTESIAN_POINT('Origin',(-1.80890829501287,-0.07938,0.658388775901912));
#13825=CARTESIAN_POINT('Origin',(-1.80890829501287,0.,0.658388775901912));
#13826=CARTESIAN_POINT('',(-1.8754727744327,-0.07938,0.258823997855139));
#13827=CARTESIAN_POINT('Ctrl Pts',(-1.8754727744327,-0.07938,0.258823997855138));
#13828=CARTESIAN_POINT('Ctrl Pts',(-1.87429319564052,-0.123392992551698,
0.267371381128541));
#13829=CARTESIAN_POINT('Ctrl Pts',(-1.87207293588642,-0.166529565724165,
0.283268822605344));
#13830=CARTESIAN_POINT('Ctrl Pts',(-1.86551115062085,-0.237213819614884,
0.323392218961362));
#13831=CARTESIAN_POINT('Ctrl Pts',(-1.86166224891746,-0.266247928944116,
0.34532483272118));
#13832=CARTESIAN_POINT('Ctrl Pts',(-1.85170818356893,-0.317173992396757,
0.395237108747477));
#13833=CARTESIAN_POINT('Ctrl Pts',(-1.84558854251276,-0.339063173951852,
0.423216711561106));
#13834=CARTESIAN_POINT('Ctrl Pts',(-1.83135774191,-0.373566122196588,0.481006384765672));
#13835=CARTESIAN_POINT('Ctrl Pts',(-1.82255520314685,-0.388075792674377,
0.513732289895913));
#13836=CARTESIAN_POINT('Ctrl Pts',(-1.8021878073054,-0.407069005705619,
0.581160429138046));
#13837=CARTESIAN_POINT('Ctrl Pts',(-1.79059939410895,-0.411552957311693,
0.615855430396488));
#13838=CARTESIAN_POINT('Ctrl Pts',(-1.76754295572641,-0.411552957311693,
0.679202474225583));
#13839=CARTESIAN_POINT('Ctrl Pts',(-1.75411867833313,-0.407069005705619,
0.713229275562222));
#13840=CARTESIAN_POINT('Ctrl Pts',(-1.72637903628921,-0.388075792674378,
0.777974136626975));
#13841=CARTESIAN_POINT('Ctrl Pts',(-1.71208636586057,-0.373566122196588,
0.808701797248777));
#13842=CARTESIAN_POINT('Ctrl Pts',(-1.68584130567972,-0.339063173951852,
0.862118637580169));
#13843=CARTESIAN_POINT('Ctrl Pts',(-1.67254428069212,-0.317173992396757,
0.88748588628286));
#13844=CARTESIAN_POINT('Ctrl Pts',(-1.64808654453785,-0.266247928944116,
0.932119257848273));
#13845=CARTESIAN_POINT('Ctrl Pts',(-1.63693696192699,-0.237213819614884,
0.951394641067894));
#13846=CARTESIAN_POINT('Ctrl Pts',(-1.61617275903043,-0.166529565724165,
0.986348780151617));
#13847=CARTESIAN_POINT('Ctrl Pts',(-1.60765489827034,-0.123392992551698,
0.999954082314951));
#13848=CARTESIAN_POINT('Ctrl Pts',(-1.60306435598592,-0.07938,1.00725997640701));
#13849=CARTESIAN_POINT('Origin',(-1.80890829501287,-0.07938,0.658388775901912));
#13850=CARTESIAN_POINT('Origin',(0.,-0.07938,0.));
#13851=CARTESIAN_POINT('',(-1.893248,-0.0793799999999999,2.31856010319213E-16));
#13852=CARTESIAN_POINT('Origin',(0.,-0.07938,0.));
#13853=CARTESIAN_POINT('',(-1.8754727744327,-0.07938,-0.258823997855139));
#13854=CARTESIAN_POINT('Origin',(0.,-0.07938,0.));
#13855=CARTESIAN_POINT('Origin',(-1.80890829501287,-0.07938,-0.658388775901913));
#13856=CARTESIAN_POINT('Origin',(-1.80890829501287,0.,-0.658388775901913));
#13857=CARTESIAN_POINT('',(-1.60306435598592,-0.07938,-1.00725997640701));
#13858=CARTESIAN_POINT('Ctrl Pts',(-1.60306435598592,-0.07938,-1.00725997640701));
#13859=CARTESIAN_POINT('Ctrl Pts',(-1.60765489827034,-0.123392992551698,
-0.999954082314952));
#13860=CARTESIAN_POINT('Ctrl Pts',(-1.61617275903043,-0.166529565724166,
-0.986348780151617));
#13861=CARTESIAN_POINT('Ctrl Pts',(-1.63693696192699,-0.237213819614884,
-0.951394641067894));
#13862=CARTESIAN_POINT('Ctrl Pts',(-1.64808654453785,-0.266247928944116,
-0.932119257848273));
#13863=CARTESIAN_POINT('Ctrl Pts',(-1.67254428069212,-0.317173992396757,
-0.88748588628286));
#13864=CARTESIAN_POINT('Ctrl Pts',(-1.68584130567972,-0.339063173951852,
-0.862118637580169));
#13865=CARTESIAN_POINT('Ctrl Pts',(-1.71208636586057,-0.373566122196588,
-0.808701797248777));
#13866=CARTESIAN_POINT('Ctrl Pts',(-1.72637903628921,-0.388075792674377,
-0.777974136626975));
#13867=CARTESIAN_POINT('Ctrl Pts',(-1.75411867833313,-0.407069005705619,
-0.713229275562223));
#13868=CARTESIAN_POINT('Ctrl Pts',(-1.76754295572641,-0.411552957311693,
-0.679202474225584));
#13869=CARTESIAN_POINT('Ctrl Pts',(-1.79059939410895,-0.411552957311693,
-0.615855430396488));
#13870=CARTESIAN_POINT('Ctrl Pts',(-1.8021878073054,-0.407069005705619,
-0.581160429138047));
#13871=CARTESIAN_POINT('Ctrl Pts',(-1.82255520314685,-0.388075792674378,
-0.513732289895914));
#13872=CARTESIAN_POINT('Ctrl Pts',(-1.83135774191,-0.373566122196588,-0.481006384765673));
#13873=CARTESIAN_POINT('Ctrl Pts',(-1.84558854251276,-0.339063173951852,
-0.423216711561107));
#13874=CARTESIAN_POINT('Ctrl Pts',(-1.85170818356893,-0.317173992396757,
-0.395237108747477));
#13875=CARTESIAN_POINT('Ctrl Pts',(-1.86166224891746,-0.266247928944116,
-0.34532483272118));
#13876=CARTESIAN_POINT('Ctrl Pts',(-1.86551115062085,-0.237213819614884,
-0.323392218961362));
#13877=CARTESIAN_POINT('Ctrl Pts',(-1.87207293588642,-0.166529565724166,
-0.283268822605344));
#13878=CARTESIAN_POINT('Ctrl Pts',(-1.87429319564052,-0.123392992551698,
-0.267371381128542));
#13879=CARTESIAN_POINT('Ctrl Pts',(-1.8754727744327,-0.07938,-0.258823997855139));
#13880=CARTESIAN_POINT('Origin',(-1.80890829501287,-0.07938,-0.658388775901913));
#13881=CARTESIAN_POINT('Origin',(0.,-0.07938,0.));
#13882=CARTESIAN_POINT('',(-1.27032663816428,-0.07938,-1.40380134701254));
#13883=CARTESIAN_POINT('Origin',(0.,-0.07938,0.));
#13884=CARTESIAN_POINT('Origin',(-0.9625,-0.07938,-1.66709890228504));
#13885=CARTESIAN_POINT('Origin',(-0.9625,0.,-1.66709890228504));
#13886=CARTESIAN_POINT('',(-0.580564309297535,-0.07938,-1.80203581326062));
#13887=CARTESIAN_POINT('Ctrl Pts',(-0.580564309297535,-0.07938,-1.80203581326062));
#13888=CARTESIAN_POINT('Ctrl Pts',(-0.588777006905474,-0.123392992551698,
-1.79938991739155));
#13889=CARTESIAN_POINT('Ctrl Pts',(-0.60404738646464,-0.166529565724165,
-1.79444282663));
#13890=CARTESIAN_POINT('Ctrl Pts',(-0.642421776219619,-0.237213819614884,
-1.78101337496783));
#13891=CARTESIAN_POINT('Ctrl Pts',(-0.663352829527298,-0.266247928944116,
-1.77341438831889));
#13892=CARTESIAN_POINT('Ctrl Pts',(-0.71077832062033,-0.317173992396757,
-1.75494437181449));
#13893=CARTESIAN_POINT('Ctrl Pts',(-0.737270185880015,-0.339063173951852,
-1.74405909481629));
#13894=CARTESIAN_POINT('Ctrl Pts',(-0.791710751504504,-0.373566122196588,
-1.72000942061118));
#13895=CARTESIAN_POINT('Ctrl Pts',(-0.822410931786042,-0.388075792674378,
-1.70565781840267));
#13896=CARTESIAN_POINT('Ctrl Pts',(-0.885277924911194,-0.407069005705619,
-1.67389107556648));
#13897=CARTESIAN_POINT('Ctrl Pts',(-0.917433524307661,-0.411552957311693,
-1.65645399266283));
#13898=CARTESIAN_POINT('Ctrl Pts',(-0.975814475692338,-0.411552957311693,
-1.62274773466534));
#13899=CARTESIAN_POINT('Ctrl Pts',(-1.00699323215303,-0.407069005705619,
-1.60361871016591));
#13900=CARTESIAN_POINT('Ctrl Pts',(-1.06593753500724,-0.388075792674378,
-1.56505766847808));
#13901=CARTESIAN_POINT('Ctrl Pts',(-1.09371647724559,-0.373566122196588,
-1.54564633355776));
#13902=CARTESIAN_POINT('Ctrl Pts',(-1.14176438887219,-0.339063173951852,
-1.51052425783311));
#13903=CARTESIAN_POINT('Ctrl Pts',(-1.1644372479097,-0.317173992396757,
-1.49302426802369));
#13904=CARTESIAN_POINT('Ctrl Pts',(-1.20414549695735,-0.266247928944116,
-1.46118759620237));
#13905=CARTESIAN_POINT('Ctrl Pts',(-1.22119193909219,-0.237213819614884,
-1.44686026563443));
#13906=CARTESIAN_POINT('Ctrl Pts',(-1.25200938026802,-0.166529565724166,
-1.42034179508298));
#13907=CARTESIAN_POINT('Ctrl Pts',(-1.26392887632193,-0.123392992551698,
-1.40959080384008));
#13908=CARTESIAN_POINT('Ctrl Pts',(-1.27032663816428,-0.07938,-1.40380134701254));
#13909=CARTESIAN_POINT('Origin',(-0.9625,-0.07938,-1.66709890228504));
#13910=CARTESIAN_POINT('Origin',(0.,-0.07938,0.));
#13911=CARTESIAN_POINT('',(-0.0707805497908242,-0.07938,-1.89192444438865));
#13912=CARTESIAN_POINT('Origin',(0.,-0.07938,0.));
#13913=CARTESIAN_POINT('Origin',(0.334272742008841,-0.07938,-1.8957549245485));
#13914=CARTESIAN_POINT('Origin',(0.334272742008841,0.,-1.8957549245485));
#13915=CARTESIAN_POINT('',(0.71358822996475,-0.07938,-1.75361906569237));
#13916=CARTESIAN_POINT('Ctrl Pts',(0.71358822996475,-0.07938,-1.75361906569237));
#13917=CARTESIAN_POINT('Ctrl Pts',(0.705596189518014,-0.123392992551698,
-1.75687121212928));
#13918=CARTESIAN_POINT('Ctrl Pts',(0.690718471466876,-0.166529565724166,
-1.76289713151763));
#13919=CARTESIAN_POINT('Ctrl Pts',(0.652689698303666,-0.237213819614884,
-1.77727615696148));
#13920=CARTESIAN_POINT('Ctrl Pts',(0.631771046764578,-0.266247928944116,
-1.78490921718958));
#13921=CARTESIAN_POINT('Ctrl Pts',(0.583568715090837,-0.317173992396757,
-1.80124488173997));
#13922=CARTESIAN_POINT('Ctrl Pts',(0.556277847738351,-0.339063173951852,
-1.8099349185301));
#13923=CARTESIAN_POINT('Ctrl Pts',(0.499115122365417,-0.373566122196588,
-1.8265055202942));
#13924=CARTESIAN_POINT('Ctrl Pts',(0.466372387779211,-0.388075792674378,
-1.83524525067263));
#13925=CARTESIAN_POINT('Ctrl Pts',(0.397794208344886,-0.407069005705619,
-1.85132063808607));
#13926=CARTESIAN_POINT('Ctrl Pts',(0.361953249272519,-0.411552957311693,
-1.85863227849762));
#13927=CARTESIAN_POINT('Ctrl Pts',(0.295564880870602,-0.411552957311693,
-1.87033833905209));
#13928=CARTESIAN_POINT('Ctrl Pts',(0.259384667806906,-0.407069005705619,
-1.87572597447038));
#13929=CARTESIAN_POINT('Ctrl Pts',(0.189444152338379,-0.388075792674377,
-1.88407517030084));
#13930=CARTESIAN_POINT('Ctrl Pts',(0.155686882426711,-0.373566122196588,
-1.88706118493262));
#13931=CARTESIAN_POINT('Ctrl Pts',(0.096304011619402,-0.339063173951852,
-1.89104071625784));
#13932=CARTESIAN_POINT('Ctrl Pts',(0.0676868173249583,-0.317173992396757,
-1.89220877917518));
#13933=CARTESIAN_POINT('Ctrl Pts',(0.0168043156156251,-0.266247928944116,
-1.89334444412923));
#13934=CARTESIAN_POINT('Ctrl Pts',(-0.00546344722567807,-0.237213819614884,
-1.89332631395644));
#13935=CARTESIAN_POINT('Ctrl Pts',(-0.0461167210878748,-0.166529565724165,
-1.89282105630055));
#13936=CARTESIAN_POINT('Ctrl Pts',(-0.0621581887675344,-0.123392992551698,
-1.89224702357808));
#13937=CARTESIAN_POINT('Ctrl Pts',(-0.0707805497908242,-0.07938,-1.89192444438865));
#13938=CARTESIAN_POINT('Origin',(0.334272742008841,-0.07938,-1.8957549245485));
#13939=CARTESIAN_POINT('Origin',(0.,-0.07938,0.));
#13940=CARTESIAN_POINT('',(1.16188454446795,-0.07938,-1.49479506783723));
#13941=CARTESIAN_POINT('Origin',(0.,-0.07938,0.));
#13942=CARTESIAN_POINT('Origin',(1.47463555300403,-0.07938,-1.23736614864659));
#13943=CARTESIAN_POINT('Origin',(1.47463555300403,0.,-1.23736614864659));
#13944=CARTESIAN_POINT('',(1.67384490577674,-0.07938,-0.884664467981643));
#13945=CARTESIAN_POINT('Ctrl Pts',(1.67384490577674,-0.07938,-0.884664467981643));
#13946=CARTESIAN_POINT('Ctrl Pts',(1.66981308703787,-0.123392992551698,
-0.892292941263125));
#13947=CARTESIAN_POINT('Ctrl Pts',(1.66228948011831,-0.166529565724165,
-0.906472276148934));
#13948=CARTESIAN_POINT('Ctrl Pts',(1.64240040915267,-0.237213819614884,
-0.941931672888549));
#13949=CARTESIAN_POINT('Ctrl Pts',(1.63128222892223,-0.266247928944116,
-0.961225186280958));
#13950=CARTESIAN_POINT('Ctrl Pts',(1.60485746336717,-0.317173992396757,
-1.00472289289232));
#13951=CARTESIAN_POINT('Ctrl Pts',(1.58953729406031,-0.339063173951852,
-1.02892207867768));
#13952=CARTESIAN_POINT('Ctrl Pts',(1.55639948343386,-0.373566122196588,
-1.07835938768384));
#13953=CARTESIAN_POINT('Ctrl Pts',(1.53693488395083,-0.388075792674377,
-1.10610103367386));
#13954=CARTESIAN_POINT('Ctrl Pts',(1.49473401052622,-0.407069005705619,
-1.16249669890816));
#13955=CARTESIAN_POINT('Ctrl Pts',(1.4719780748558,-0.411552957311693,-1.19113586482651));
#13956=CARTESIAN_POINT('Ctrl Pts',(1.42864614483643,-0.411552957311693,
-1.24277684810113));
#13957=CARTESIAN_POINT('Ctrl Pts',(1.40439359896051,-0.407069005705619,
-1.27016020894803));
#13958=CARTESIAN_POINT('Ctrl Pts',(1.35618281536764,-0.388075792674378,
-1.32151296077672));
#13959=CARTESIAN_POINT('Ctrl Pts',(1.33224261954459,-0.373566122196588,
-1.34549913552853));
#13960=CARTESIAN_POINT('Ctrl Pts',(1.28931069477441,-0.339063173951852,
-1.38671820696899));
#13961=CARTESIAN_POINT('Ctrl Pts',(1.26813946847809,-0.317173992396757,
-1.40600777299249));
#13962=CARTESIAN_POINT('Ctrl Pts',(1.22989120215289,-0.266247928944116,
-1.4395843844684));
#13963=CARTESIAN_POINT('Ctrl Pts',(1.21282145231718,-0.237213819614884,
-1.45388393800011));
#13964=CARTESIAN_POINT('Ctrl Pts',(1.18135446441955,-0.166529565724166,
-1.47962830891229));
#13965=CARTESIAN_POINT('Ctrl Pts',(1.16869700612251,-0.123392992551698,
-1.48949983100074));
#13966=CARTESIAN_POINT('Ctrl Pts',(1.16188454446795,-0.0793799999999999,
-1.49479506783723));
#13967=CARTESIAN_POINT('Origin',(1.47463555300403,-0.07938,-1.23736614864659));
#13968=CARTESIAN_POINT('Origin',(0.,-0.27783,0.));
#13969=CARTESIAN_POINT('',(-1.893248,-0.47628,2.31856010319213E-16));
#13970=CARTESIAN_POINT('Origin',(0.,-0.47628,0.));
#13971=CARTESIAN_POINT('',(-1.893248,-0.27783,2.31856010319213E-16));
#13972=CARTESIAN_POINT('',(1.85089094746182,-0.07938,0.39823446624808));
#13973=CARTESIAN_POINT('Origin',(0.,-0.07938,0.));
#13974=CARTESIAN_POINT('',(1.85089094746182,-0.07938,-0.39823446624808));
#13975=CARTESIAN_POINT('Ctrl Pts',(1.85089094746182,-0.07938,0.39823446624808));
#13976=CARTESIAN_POINT('Ctrl Pts',(1.8527058832274,-0.123392992551698,0.38979911355147));
#13977=CARTESIAN_POINT('Ctrl Pts',(1.85605676673266,-0.166529565724166,
0.374101031547026));
#13978=CARTESIAN_POINT('Ctrl Pts',(1.86361371531181,-0.237213819614884,
0.334153109333404));
#13979=CARTESIAN_POINT('Ctrl Pts',(1.86749832648465,-0.266247928944116,
0.312226792116516));
#13980=CARTESIAN_POINT('Ctrl Pts',(1.87521556853004,-0.317173992396757,
0.261920103790797));
#13981=CARTESIAN_POINT('Ctrl Pts',(1.87903457475221,-0.339063173951852,
0.233534836983177));
#13982=CARTESIAN_POINT('Ctrl Pts',(1.88542722875009,-0.373566122196588,
0.174363087053423));
#13983=CARTESIAN_POINT('Ctrl Pts',(1.88834846679328,-0.388075792674378,
0.140600149924591));
#13984=CARTESIAN_POINT('Ctrl Pts',(1.89227115706422,-0.407069005705619,
0.0702723654005715));
#13985=CARTESIAN_POINT('Ctrl Pts',(1.893248,-0.411552957311693,0.0337062579974903));
#13986=CARTESIAN_POINT('Ctrl Pts',(1.893248,-0.411552957311693,-0.0337062579974903));
#13987=CARTESIAN_POINT('Ctrl Pts',(1.89227115706422,-0.407069005705619,
-0.0702723654005715));
#13988=CARTESIAN_POINT('Ctrl Pts',(1.88834846679328,-0.388075792674378,
-0.140600149924591));
#13989=CARTESIAN_POINT('Ctrl Pts',(1.88542722875009,-0.373566122196588,
-0.174363087053422));
#13990=CARTESIAN_POINT('Ctrl Pts',(1.87903457475221,-0.339063173951852,
-0.233534836983177));
#13991=CARTESIAN_POINT('Ctrl Pts',(1.87521556853004,-0.317173992396757,
-0.261920103790797));
#13992=CARTESIAN_POINT('Ctrl Pts',(1.86749832648465,-0.266247928944116,
-0.312226792116516));
#13993=CARTESIAN_POINT('Ctrl Pts',(1.86361371531181,-0.237213819614884,
-0.334153109333404));
#13994=CARTESIAN_POINT('Ctrl Pts',(1.85605676673266,-0.166529565724166,
-0.374101031547026));
#13995=CARTESIAN_POINT('Ctrl Pts',(1.8527058832274,-0.123392992551698,-0.38979911355147));
#13996=CARTESIAN_POINT('Ctrl Pts',(1.85089094746182,-0.07938,-0.39823446624808));
#13997=CARTESIAN_POINT('Origin',(0.,-0.07938,0.));
#13998=CARTESIAN_POINT('Origin',(0.,-0.07938,0.));
#13999=CARTESIAN_POINT('Origin',(1.925,-0.07938,0.));
#14000=CARTESIAN_POINT('Origin',(1.925,0.,0.));
#14001=CARTESIAN_POINT('Origin',(1.925,-0.07938,0.));
#14002=CARTESIAN_POINT('Origin',(0.,-0.47628,0.));
#14003=CARTESIAN_POINT('Origin',(0.,-0.07938,0.));
#14004=CARTESIAN_POINT('',(0.,0.,0.));
#14005=CARTESIAN_POINT('Origin',(1.95469,0.745,0.));
#14006=CARTESIAN_POINT('',(-1.95469,0.745,-2.39380485182534E-16));
#14007=CARTESIAN_POINT('Origin',(0.,0.745,0.));
#14008=CARTESIAN_POINT('',(-1.90031,0.745,-2.32720855888771E-16));
#14009=CARTESIAN_POINT('Origin',(0.,0.745,0.));
#14010=CARTESIAN_POINT('Origin',(0.,0.7075,0.));
#14011=CARTESIAN_POINT('',(-1.95469,0.67,-2.39380485182534E-16));
#14012=CARTESIAN_POINT('Origin',(0.,0.67,0.));
#14013=CARTESIAN_POINT('',(-1.95469,0.7075,-2.39380485182534E-16));
#14014=CARTESIAN_POINT('Origin',(1.90031,0.67,0.));
#14015=CARTESIAN_POINT('',(-1.90031,0.67,-2.32720855888771E-16));
#14016=CARTESIAN_POINT('Origin',(0.,0.67,0.));
#14017=CARTESIAN_POINT('Origin',(0.,0.7075,0.));
#14018=CARTESIAN_POINT('',(-1.90031,0.7075,-2.32720855888771E-16));
#14019=CARTESIAN_POINT('Origin',(1.95469,-0.67,0.));
#14020=CARTESIAN_POINT('',(-1.95469,-0.67,-2.39380485182534E-16));
#14021=CARTESIAN_POINT('Origin',(0.,-0.67,0.));
#14022=CARTESIAN_POINT('',(-1.90031,-0.67,-2.32720855888771E-16));
#14023=CARTESIAN_POINT('Origin',(0.,-0.67,0.));
#14024=CARTESIAN_POINT('Origin',(0.,-0.7075,0.));
#14025=CARTESIAN_POINT('',(-1.95469,-0.745,-2.39380485182534E-16));
#14026=CARTESIAN_POINT('Origin',(0.,-0.745,0.));
#14027=CARTESIAN_POINT('',(-1.95469,-0.7075,-2.39380485182534E-16));
#14028=CARTESIAN_POINT('Origin',(1.90031,-0.745,0.));
#14029=CARTESIAN_POINT('',(-1.90031,-0.745,-2.32720855888771E-16));
#14030=CARTESIAN_POINT('Origin',(0.,-0.745,0.));
#14031=CARTESIAN_POINT('Origin',(0.,-0.7075,0.));
#14032=CARTESIAN_POINT('',(-1.90031,-0.7075,-2.32720855888771E-16));
#14033=CARTESIAN_POINT('',(0.,0.,0.));
#14034=CARTESIAN_POINT('',(0.,0.,0.));
#14035=CARTESIAN_POINT('',(0.,0.,0.));
#14036=CARTESIAN_POINT('',(0.,0.,0.));
#14037=CARTESIAN_POINT('',(0.,0.,0.));
#14038=CARTESIAN_POINT('',(0.,0.,0.));
#14039=CARTESIAN_POINT('Origin',(-18.,21.,-0.6));
#14040=CARTESIAN_POINT('',(-18.,21.,-0.6));
#14041=CARTESIAN_POINT('',(-20.,21.,-0.6));
#14042=CARTESIAN_POINT('',(-18.,21.,-0.6));
#14043=CARTESIAN_POINT('',(-20.,21.,0.));
#14044=CARTESIAN_POINT('',(-20.,21.,-0.6));
#14045=CARTESIAN_POINT('',(-18.,21.,0.));
#14046=CARTESIAN_POINT('',(-18.,21.,0.));
#14047=CARTESIAN_POINT('',(-18.,21.,-0.6));
#14048=CARTESIAN_POINT('Origin',(-18.,-21.,-0.6));
#14049=CARTESIAN_POINT('',(-18.,-21.,-0.6));
#14050=CARTESIAN_POINT('',(-18.,-21.,-0.6));
#14051=CARTESIAN_POINT('',(-18.,-21.,0.));
#14052=CARTESIAN_POINT('',(-18.,-21.,0.));
#14053=CARTESIAN_POINT('',(-18.,-21.,-0.6));
#14054=CARTESIAN_POINT('Origin',(-20.,-21.,-0.6));
#14055=CARTESIAN_POINT('',(-20.,-21.,-0.6));
#14056=CARTESIAN_POINT('',(-20.,-21.,-0.6));
#14057=CARTESIAN_POINT('',(-20.,-21.,0.));
#14058=CARTESIAN_POINT('',(-20.,-21.,0.));
#14059=CARTESIAN_POINT('',(-20.,-21.,-0.6));
#14060=CARTESIAN_POINT('Origin',(-20.,21.,-0.6));
#14061=CARTESIAN_POINT('',(-20.,21.,-0.6));
#14062=CARTESIAN_POINT('',(-20.,21.,0.));
#14063=CARTESIAN_POINT('Origin',(-19.,0.,0.));
#14064=CARTESIAN_POINT('Origin',(-19.,0.,-0.6));
#14065=CARTESIAN_POINT('',(0.,0.,0.));
#14066=CARTESIAN_POINT('Origin',(20.,21.,-0.6));
#14067=CARTESIAN_POINT('',(20.,21.,-0.6));
#14068=CARTESIAN_POINT('',(18.,21.,-0.6));
#14069=CARTESIAN_POINT('',(20.,21.,-0.6));
#14070=CARTESIAN_POINT('',(18.,21.,0.));
#14071=CARTESIAN_POINT('',(18.,21.,-0.6));
#14072=CARTESIAN_POINT('',(20.,21.,0.));
#14073=CARTESIAN_POINT('',(20.,21.,0.));
#14074=CARTESIAN_POINT('',(20.,21.,-0.6));
#14075=CARTESIAN_POINT('Origin',(20.,-21.,-0.6));
#14076=CARTESIAN_POINT('',(20.,-21.,-0.6));
#14077=CARTESIAN_POINT('',(20.,-21.,-0.6));
#14078=CARTESIAN_POINT('',(20.,-21.,0.));
#14079=CARTESIAN_POINT('',(20.,-21.,0.));
#14080=CARTESIAN_POINT('',(20.,-21.,-0.6));
#14081=CARTESIAN_POINT('Origin',(18.,-21.,-0.6));
#14082=CARTESIAN_POINT('',(18.,-21.,-0.6));
#14083=CARTESIAN_POINT('',(18.,-21.,-0.6));
#14084=CARTESIAN_POINT('',(18.,-21.,0.));
#14085=CARTESIAN_POINT('',(18.,-21.,0.));
#14086=CARTESIAN_POINT('',(18.,-21.,-0.6));
#14087=CARTESIAN_POINT('Origin',(18.,21.,-0.6));
#14088=CARTESIAN_POINT('',(18.,21.,-0.6));
#14089=CARTESIAN_POINT('',(18.,21.,0.));
#14090=CARTESIAN_POINT('Origin',(19.,0.,0.));
#14091=CARTESIAN_POINT('Origin',(19.,0.,-0.6));
#14092=CARTESIAN_POINT('',(0.,0.,0.));
#14093=CARTESIAN_POINT('',(0.,0.,0.));
#14094=CARTESIAN_POINT('Origin',(1.2,0.,4.3));
#14095=CARTESIAN_POINT('',(1.035,-2.02066721859313E-17,4.3));
#14096=CARTESIAN_POINT('Origin',(1.2,0.,4.3));
#14097=CARTESIAN_POINT('',(1.035,2.02066721859313E-17,5.5));
#14098=CARTESIAN_POINT('',(1.035,-2.02066721859313E-17,4.3));
#14099=CARTESIAN_POINT('Origin',(1.2,0.,5.5));
#14100=CARTESIAN_POINT('Origin',(1.2,0.,4.3));
#14101=CARTESIAN_POINT('Origin',(-0.6,1.03923048454133,4.3));
#14102=CARTESIAN_POINT('',(-0.765,1.03923048454133,4.3));
#14103=CARTESIAN_POINT('Origin',(-0.6,1.03923048454133,4.3));
#14104=CARTESIAN_POINT('',(-0.765,1.03923048454133,5.5));
#14105=CARTESIAN_POINT('',(-0.765,1.03923048454133,4.3));
#14106=CARTESIAN_POINT('Origin',(-0.6,1.03923048454133,5.5));
#14107=CARTESIAN_POINT('Origin',(-0.6,1.03923048454133,4.3));
#14108=CARTESIAN_POINT('Origin',(-0.600000000000001,-1.03923048454133,4.3));
#14109=CARTESIAN_POINT('',(-0.765000000000001,-1.03923048454133,4.3));
#14110=CARTESIAN_POINT('Origin',(-0.600000000000001,-1.03923048454133,4.3));
#14111=CARTESIAN_POINT('',(-0.765000000000001,-1.03923048454133,5.5));
#14112=CARTESIAN_POINT('',(-0.765000000000001,-1.03923048454133,4.3));
#14113=CARTESIAN_POINT('Origin',(-0.600000000000001,-1.03923048454133,5.5));
#14114=CARTESIAN_POINT('Origin',(-0.600000000000001,-1.03923048454133,4.3));
#14115=CARTESIAN_POINT('Origin',(0.,0.,4.25));
#14116=CARTESIAN_POINT('',(-1.75,-2.14313189850787E-16,4.25));
#14117=CARTESIAN_POINT('Origin',(0.,0.,4.25));
#14118=CARTESIAN_POINT('',(-1.25,1.53080849893419E-16,4.25));
#14119=CARTESIAN_POINT('Origin',(0.,0.,4.25));
#14120=CARTESIAN_POINT('Origin',(0.,0.,4.25));
#14121=CARTESIAN_POINT('',(-1.75,-2.14313189850787E-16,5.5));
#14122=CARTESIAN_POINT('Origin',(0.,0.,5.5));
#14123=CARTESIAN_POINT('',(-1.75,-2.14313189850787E-16,4.25));
#14124=CARTESIAN_POINT('Origin',(0.,0.,2.));
#14125=CARTESIAN_POINT('',(-1.25,-1.53080849893419E-16,2.));
#14126=CARTESIAN_POINT('',(-1.25,-1.53080849893419E-16,2.));
#14127=CARTESIAN_POINT('Origin',(0.,0.,2.));
#14128=CARTESIAN_POINT('Origin',(0.,0.,5.5));
#14129=CARTESIAN_POINT('Origin',(0.,0.,2.));
#14130=CARTESIAN_POINT('',(0.,0.,0.));
#14131=CARTESIAN_POINT('Origin',(1.2,0.,5.4));
#14132=CARTESIAN_POINT('',(0.975,-2.75545529808155E-17,5.5));
#14133=CARTESIAN_POINT('Origin',(1.2,0.,5.5));
#14134=CARTESIAN_POINT('',(0.975,2.75545529808155E-17,6.7));
#14135=CARTESIAN_POINT('',(0.975,-2.75545529808155E-17,5.4));
#14136=CARTESIAN_POINT('Origin',(1.2,0.,6.7));
#14137=CARTESIAN_POINT('Origin',(-0.6,1.03923048454133,5.4));
#14138=CARTESIAN_POINT('',(-0.825,1.03923048454133,5.5));
#14139=CARTESIAN_POINT('Origin',(-0.6,1.03923048454133,5.5));
#14140=CARTESIAN_POINT('',(-0.825,1.03923048454133,6.7));
#14141=CARTESIAN_POINT('',(-0.825,1.03923048454133,5.4));
#14142=CARTESIAN_POINT('Origin',(-0.6,1.03923048454133,6.7));
#14143=CARTESIAN_POINT('Origin',(-0.600000000000001,-1.03923048454133,5.4));
#14144=CARTESIAN_POINT('',(-0.825000000000001,-1.03923048454133,5.5));
#14145=CARTESIAN_POINT('Origin',(-0.600000000000001,-1.03923048454133,5.5));
#14146=CARTESIAN_POINT('',(-0.825000000000001,-1.03923048454133,6.7));
#14147=CARTESIAN_POINT('',(-0.825000000000001,-1.03923048454133,5.4));
#14148=CARTESIAN_POINT('Origin',(-0.600000000000001,-1.03923048454133,6.7));
#14149=CARTESIAN_POINT('Origin',(7.,0.,5.4));
#14150=CARTESIAN_POINT('',(6.75,-3.06161699786838E-17,5.5));
#14151=CARTESIAN_POINT('Origin',(7.,0.,5.5));
#14152=CARTESIAN_POINT('',(6.75,3.06161699786838E-17,6.7));
#14153=CARTESIAN_POINT('',(6.75,-3.06161699786838E-17,5.4));
#14154=CARTESIAN_POINT('Origin',(7.,0.,6.7));
#14155=CARTESIAN_POINT('Origin',(0.,7.,5.4));
#14156=CARTESIAN_POINT('',(-0.25,7.,5.5));
#14157=CARTESIAN_POINT('Origin',(0.,7.,5.5));
#14158=CARTESIAN_POINT('',(-0.25,7.,6.7));
#14159=CARTESIAN_POINT('',(-0.25,7.,5.4));
#14160=CARTESIAN_POINT('Origin',(0.,7.,6.7));
#14161=CARTESIAN_POINT('Origin',(0.,0.,5.4));
#14162=CARTESIAN_POINT('',(-0.25,-3.06161699786838E-17,5.5));
#14163=CARTESIAN_POINT('Origin',(0.,0.,5.5));
#14164=CARTESIAN_POINT('',(-0.25,3.06161699786838E-17,6.7));
#14165=CARTESIAN_POINT('',(-0.25,-3.06161699786838E-17,5.4));
#14166=CARTESIAN_POINT('Origin',(0.,0.,6.7));
#14167=CARTESIAN_POINT('Origin',(-7.,7.,5.4));
#14168=CARTESIAN_POINT('',(-7.25,7.,5.5));
#14169=CARTESIAN_POINT('Origin',(-7.,7.,5.5));
#14170=CARTESIAN_POINT('',(-7.25,7.,6.7));
#14171=CARTESIAN_POINT('',(-7.25,7.,5.4));
#14172=CARTESIAN_POINT('Origin',(-7.,7.,6.7));
#14173=CARTESIAN_POINT('Origin',(-7.,0.,5.4));
#14174=CARTESIAN_POINT('',(-7.25,-3.06161699786838E-17,5.5));
#14175=CARTESIAN_POINT('Origin',(-7.,0.,5.5));
#14176=CARTESIAN_POINT('',(-7.25,3.06161699786838E-17,6.7));
#14177=CARTESIAN_POINT('',(-7.25,-3.06161699786838E-17,5.4));
#14178=CARTESIAN_POINT('Origin',(-7.,0.,6.7));
#14179=CARTESIAN_POINT('Origin',(0.,-7.,5.4));
#14180=CARTESIAN_POINT('',(-0.25,-7.,5.5));
#14181=CARTESIAN_POINT('Origin',(0.,-7.,5.5));
#14182=CARTESIAN_POINT('',(-0.25,-7.,6.7));
#14183=CARTESIAN_POINT('',(-0.25,-7.,5.4));
#14184=CARTESIAN_POINT('Origin',(0.,-7.,6.7));
#14185=CARTESIAN_POINT('Origin',(-7.,-7.,5.4));
#14186=CARTESIAN_POINT('',(-7.25,-7.,5.5));
#14187=CARTESIAN_POINT('Origin',(-7.,-7.,5.5));
#14188=CARTESIAN_POINT('',(-7.25,-7.,6.7));
#14189=CARTESIAN_POINT('',(-7.25,-7.,5.4));
#14190=CARTESIAN_POINT('Origin',(-7.,-7.,6.7));
#14191=CARTESIAN_POINT('Origin',(7.,-7.,5.4));
#14192=CARTESIAN_POINT('',(6.75,-7.,5.5));
#14193=CARTESIAN_POINT('Origin',(7.,-7.,5.5));
#14194=CARTESIAN_POINT('',(6.75,-7.,6.7));
#14195=CARTESIAN_POINT('',(6.75,-7.,5.4));
#14196=CARTESIAN_POINT('Origin',(7.,-7.,6.7));
#14197=CARTESIAN_POINT('Origin',(7.,7.,5.4));
#14198=CARTESIAN_POINT('',(6.75,7.,5.5));
#14199=CARTESIAN_POINT('Origin',(7.,7.,5.5));
#14200=CARTESIAN_POINT('',(6.75,7.,6.7));
#14201=CARTESIAN_POINT('',(6.75,7.,5.4));
#14202=CARTESIAN_POINT('Origin',(7.,7.,6.7));
#14203=CARTESIAN_POINT('Origin',(0.,0.,5.5));
#14204=CARTESIAN_POINT('',(-20.,-2.44929359829471E-15,6.7));
#14205=CARTESIAN_POINT('Origin',(0.,0.,6.7));
#14206=CARTESIAN_POINT('',(-20.,-2.44929359829471E-15,5.5));
#14207=CARTESIAN_POINT('',(-20.,-2.44929359829471E-15,5.5));
#14208=CARTESIAN_POINT('Origin',(0.,0.,5.5));
#14209=CARTESIAN_POINT('Origin',(0.,0.,6.7));
#14210=CARTESIAN_POINT('Origin',(0.,0.,5.5));
#14211=CARTESIAN_POINT('',(0.,0.,0.));
#14212=CARTESIAN_POINT('Origin',(0.,1.24,2.4));
#14213=CARTESIAN_POINT('',(-0.193455421221531,1.24,2.31829932680816));
#14214=CARTESIAN_POINT('',(-0.193455421221531,1.24,2.48170067319184));
#14215=CARTESIAN_POINT('',(-0.193455421221531,1.24,2.));
#14216=CARTESIAN_POINT('',(-0.21,1.24,2.4));
#14217=CARTESIAN_POINT('Origin',(0.,1.24,2.4));
#14218=CARTESIAN_POINT('Origin',(0.,1.24,2.4));
#14219=CARTESIAN_POINT('Origin',(0.,1.24,2.4));
#14220=CARTESIAN_POINT('',(0.193455421221531,1.24,2.31829932680816));
#14221=CARTESIAN_POINT('Ctrl Pts',(0.19345542122153,1.24,2.31829932680816));
#14222=CARTESIAN_POINT('Ctrl Pts',(0.182741806873435,1.24167145707784,2.29293103184137));
#14223=CARTESIAN_POINT('Ctrl Pts',(0.16680484953796,1.24400210952839,2.26982000143961));
#14224=CARTESIAN_POINT('Ctrl Pts',(0.129875785635208,1.24840249136865,2.23289093753686));
#14225=CARTESIAN_POINT('Ctrl Pts',(0.106295060941802,1.2507589672592,2.2167372734261));
#14226=CARTESIAN_POINT('Ctrl Pts',(0.0545698089447938,1.25408084670822,
2.19529044194989));
#14227=CARTESIAN_POINT('Ctrl Pts',(0.0264211917910691,1.255,2.19));
#14228=CARTESIAN_POINT('Ctrl Pts',(-0.0264211917910689,1.255,2.19));
#14229=CARTESIAN_POINT('Ctrl Pts',(-0.0545698089447936,1.25408084670822,
2.19529044194989));
#14230=CARTESIAN_POINT('Ctrl Pts',(-0.106295060941802,1.2507589672592,2.2167372734261));
#14231=CARTESIAN_POINT('Ctrl Pts',(-0.129875785635207,1.24840249136865,
2.23289093753686));
#14232=CARTESIAN_POINT('Ctrl Pts',(-0.16680484953796,1.24400210952839,2.26982000143961));
#14233=CARTESIAN_POINT('Ctrl Pts',(-0.182741806873435,1.24167145707784,
2.29293103184137));
#14234=CARTESIAN_POINT('Ctrl Pts',(-0.193455421221531,1.24,2.31829932680816));
#14235=CARTESIAN_POINT('',(0.193455421221531,1.24,2.48170067319184));
#14236=CARTESIAN_POINT('Origin',(0.,1.24,2.4));
#14237=CARTESIAN_POINT('Ctrl Pts',(-0.193455421221531,1.24,2.48170067319184));
#14238=CARTESIAN_POINT('Ctrl Pts',(-0.182741806873435,1.24167145707784,
2.50706896815863));
#14239=CARTESIAN_POINT('Ctrl Pts',(-0.16680484953796,1.24400210952839,2.53017999856039));
#14240=CARTESIAN_POINT('Ctrl Pts',(-0.129875785635208,1.24840249136865,
2.56710906246314));
#14241=CARTESIAN_POINT('Ctrl Pts',(-0.106295060941802,1.2507589672592,2.5832627265739));
#14242=CARTESIAN_POINT('Ctrl Pts',(-0.0545698089447938,1.25408084670822,
2.6047095580501));
#14243=CARTESIAN_POINT('Ctrl Pts',(-0.0264211917910691,1.255,2.61));
#14244=CARTESIAN_POINT('Ctrl Pts',(0.026421191791069,1.255,2.61));
#14245=CARTESIAN_POINT('Ctrl Pts',(0.0545698089447936,1.25408084670822,
2.60470955805011));
#14246=CARTESIAN_POINT('Ctrl Pts',(0.106295060941802,1.2507589672592,2.5832627265739));
#14247=CARTESIAN_POINT('Ctrl Pts',(0.129875785635207,1.24840249136865,2.56710906246314));
#14248=CARTESIAN_POINT('Ctrl Pts',(0.16680484953796,1.24400210952839,2.53017999856039));
#14249=CARTESIAN_POINT('Ctrl Pts',(0.182741806873434,1.24167145707784,2.50706896815863));
#14250=CARTESIAN_POINT('Ctrl Pts',(0.19345542122153,1.24,2.48170067319184));
#14251=CARTESIAN_POINT('',(-0.21,1.78770802985275,2.4));
#14252=CARTESIAN_POINT('',(-0.21,1.24,2.4));
#14253=CARTESIAN_POINT('Ctrl Pts',(-0.21,1.78770802985275,2.4));
#14254=CARTESIAN_POINT('Ctrl Pts',(-0.21,1.78770802985275,2.37360603148425));
#14255=CARTESIAN_POINT('Ctrl Pts',(-0.204720232951726,1.78835284034214,
2.34546934556602));
#14256=CARTESIAN_POINT('Ctrl Pts',(-0.183281523978899,1.79067700538683,
2.29373688397397));
#14257=CARTESIAN_POINT('Ctrl Pts',(-0.167123888882363,1.79232226897314,
2.27013904078401));
#14258=CARTESIAN_POINT('Ctrl Pts',(-0.129861077103665,1.79540680803063,
2.23287622900532));
#14259=CARTESIAN_POINT('Ctrl Pts',(-0.106263182528071,1.79704717240673,
2.2167185016358));
#14260=CARTESIAN_POINT('Ctrl Pts',(-0.0545305475112074,1.79936011492601,
2.19527972468261));
#14261=CARTESIAN_POINT('Ctrl Pts',(-0.0263938015120406,1.8,2.19));
#14262=CARTESIAN_POINT('Ctrl Pts',(0.0263938015120407,1.8,2.19));
#14263=CARTESIAN_POINT('Ctrl Pts',(0.0545305475112074,1.79936011492601,
2.19527972468261));
#14264=CARTESIAN_POINT('Ctrl Pts',(0.106263182528071,1.79704717240673,2.2167185016358));
#14265=CARTESIAN_POINT('Ctrl Pts',(0.129861077103665,1.79540680803063,2.23287622900532));
#14266=CARTESIAN_POINT('Ctrl Pts',(0.167123888882363,1.79232226897314,2.27013904078401));
#14267=CARTESIAN_POINT('Ctrl Pts',(0.183281523978899,1.79067700538683,2.29373688397397));
#14268=CARTESIAN_POINT('Ctrl Pts',(0.204720232951726,1.78835284034214,2.34546934556602));
#14269=CARTESIAN_POINT('Ctrl Pts',(0.21,1.78770802985275,2.37360603148425));
#14270=CARTESIAN_POINT('Ctrl Pts',(0.21,1.78770802985275,2.42639396851575));
#14271=CARTESIAN_POINT('Ctrl Pts',(0.204720232951726,1.78835284034214,2.45453065443398));
#14272=CARTESIAN_POINT('Ctrl Pts',(0.183281523978899,1.79067700538683,2.50626311602603));
#14273=CARTESIAN_POINT('Ctrl Pts',(0.167123888882363,1.79232226897314,2.52986095921599));
#14274=CARTESIAN_POINT('Ctrl Pts',(0.129861077103665,1.79540680803063,2.56712377099468));
#14275=CARTESIAN_POINT('Ctrl Pts',(0.106263182528071,1.79704717240673,2.5832814983642));
#14276=CARTESIAN_POINT('Ctrl Pts',(0.0545305475112074,1.79936011492601,
2.60472027531739));
#14277=CARTESIAN_POINT('Ctrl Pts',(0.0263938015120407,1.8,2.61));
#14278=CARTESIAN_POINT('Ctrl Pts',(-0.0263938015120406,1.8,2.61));
#14279=CARTESIAN_POINT('Ctrl Pts',(-0.0545305475112074,1.79936011492601,
2.60472027531739));
#14280=CARTESIAN_POINT('Ctrl Pts',(-0.106263182528071,1.79704717240673,
2.5832814983642));
#14281=CARTESIAN_POINT('Ctrl Pts',(-0.129861077103665,1.79540680803063,
2.56712377099468));
#14282=CARTESIAN_POINT('Ctrl Pts',(-0.167123888882363,1.79232226897314,
2.52986095921599));
#14283=CARTESIAN_POINT('Ctrl Pts',(-0.183281523978899,1.79067700538683,
2.50626311602603));
#14284=CARTESIAN_POINT('Ctrl Pts',(-0.204720232951726,1.78835284034214,
2.45453065443398));
#14285=CARTESIAN_POINT('Ctrl Pts',(-0.21,1.78770802985275,2.42639396851575));
#14286=CARTESIAN_POINT('Ctrl Pts',(-0.21,1.78770802985275,2.4));
#14287=CARTESIAN_POINT('Origin',(0.,1.24,2.4));
#14288=CARTESIAN_POINT('',(0.193455421221531,1.24,2.));
#14289=CARTESIAN_POINT('Origin',(0.,0.,2.));
#14290=CARTESIAN_POINT('',(-1.255,-1.53693173292993E-16,2.75));
#14291=CARTESIAN_POINT('Origin',(0.,0.,2.75));
#14292=CARTESIAN_POINT('',(-1.255,-1.53693173292993E-16,2.));
#14293=CARTESIAN_POINT('',(-1.255,-1.53693173292993E-16,2.));
#14294=CARTESIAN_POINT('Origin',(0.,0.,2.));
#14295=CARTESIAN_POINT('Origin',(0.,0.,2.));
#14296=CARTESIAN_POINT('',(-1.8,-2.20436423846524E-16,2.75));
#14297=CARTESIAN_POINT('Origin',(0.,0.,2.75));
#14298=CARTESIAN_POINT('',(-1.8,-2.20436423846524E-16,2.));
#14299=CARTESIAN_POINT('',(-1.8,-2.20436423846524E-16,2.));
#14300=CARTESIAN_POINT('Origin',(0.,0.,2.));
#14301=CARTESIAN_POINT('Origin',(0.,0.,2.75));
#14302=CARTESIAN_POINT('Origin',(0.,0.,2.));
#14303=CARTESIAN_POINT('',(0.,0.,0.));
#14304=CARTESIAN_POINT('Origin',(0.3,0.4,0.));
#14305=CARTESIAN_POINT('',(-0.3,0.4,-3.67394039744206E-17));
#14306=CARTESIAN_POINT('Origin',(0.,0.4,0.));
#14307=CARTESIAN_POINT('Origin',(0.,0.375,0.));
#14308=CARTESIAN_POINT('',(-0.35,0.35,-4.28626379701573E-17));
#14309=CARTESIAN_POINT('Origin',(0.,0.35,0.));
#14310=CARTESIAN_POINT('',(-0.325,0.375,-3.9801020972289E-17));
#14311=CARTESIAN_POINT('Origin',(0.,0.19,0.));
#14312=CARTESIAN_POINT('',(-0.35,0.03,-4.28626379701574E-17));
#14313=CARTESIAN_POINT('Origin',(0.,0.03,0.));
#14314=CARTESIAN_POINT('',(-0.35,0.19,-4.28626379701574E-17));
#14315=CARTESIAN_POINT('Origin',(0.,0.0149999999999999,0.));
#14316=CARTESIAN_POINT('',(-0.32,-3.29597460435593E-17,-3.91886975727153E-17));
#14317=CARTESIAN_POINT('Origin',(0.,0.,0.));
#14318=CARTESIAN_POINT('',(-0.335,0.0149999999999999,-4.10256677714363E-17));
#14319=CARTESIAN_POINT('Origin',(0.22,0.,0.));
#14320=CARTESIAN_POINT('',(-0.22,-6.93889390390723E-18,-2.69422295812418E-17));
#14321=CARTESIAN_POINT('Origin',(0.,0.,0.));
#14322=CARTESIAN_POINT('Origin',(0.,-0.02,0.));
#14323=CARTESIAN_POINT('',(-0.1954,-0.0492,2.39295984553393E-17));
#14324=CARTESIAN_POINT('Origin',(0.,-0.0492,0.));
#14325=CARTESIAN_POINT('',(-0.21,-0.02,-2.57175827820944E-17));
#14326=CARTESIAN_POINT('Origin',(0.,-0.8,0.));
#14327=CARTESIAN_POINT('',(-0.1954,-1.5646,2.39295984553393E-17));
#14328=CARTESIAN_POINT('Origin',(0.,-1.5646,0.));
#14329=CARTESIAN_POINT('',(-0.1954,-0.8,-2.39295984553393E-17));
#14330=CARTESIAN_POINT('Origin',(0.,-1.58,0.));
#14331=CARTESIAN_POINT('',(-0.16,-1.6,-1.95943487863577E-17));
#14332=CARTESIAN_POINT('Origin',(0.,-1.6,0.));
#14333=CARTESIAN_POINT('',(-0.18,-1.58,-2.20436423846524E-17));
#14334=CARTESIAN_POINT('Origin',(0.,-1.6,0.));
#14335=CARTESIAN_POINT('Origin',(0.0866025403784439,-0.4,-0.15));
#14336=CARTESIAN_POINT('',(0.173205080756888,-0.4,0.));
#14337=CARTESIAN_POINT('',(0.0866025403784439,-0.4,-0.15));
#14338=CARTESIAN_POINT('',(0.173205080756888,-0.4,0.));
#14339=CARTESIAN_POINT('',(0.0866025403784439,-0.64,-0.15));
#14340=CARTESIAN_POINT('',(0.0866025403784439,-0.4,-0.15));
#14341=CARTESIAN_POINT('',(0.173205080756888,-0.64,0.));
#14342=CARTESIAN_POINT('',(0.173205080756888,-0.64,0.));
#14343=CARTESIAN_POINT('',(0.173205080756888,-0.4,0.));
#14344=CARTESIAN_POINT('Origin',(-0.0866025403784438,-0.4,-0.15));
#14345=CARTESIAN_POINT('',(-0.0866025403784438,-0.4,-0.15));
#14346=CARTESIAN_POINT('',(0.0866025403784439,-0.4,-0.15));
#14347=CARTESIAN_POINT('',(-0.0866025403784438,-0.64,-0.15));
#14348=CARTESIAN_POINT('',(-0.0866025403784438,-0.4,-0.15));
#14349=CARTESIAN_POINT('',(0.0866025403784439,-0.64,-0.15));
#14350=CARTESIAN_POINT('Origin',(-0.173205080756888,-0.4,-2.77555756156289E-17));
#14351=CARTESIAN_POINT('',(-0.173205080756888,-0.4,-2.12115047744981E-17));
#14352=CARTESIAN_POINT('',(-0.0866025403784438,-0.4,-0.15));
#14353=CARTESIAN_POINT('',(-0.173205080756888,-0.64,-2.77555756156289E-17));
#14354=CARTESIAN_POINT('',(-0.173205080756888,-0.4,-2.12115047744981E-17));
#14355=CARTESIAN_POINT('',(-0.0866025403784438,-0.64,-0.15));
#14356=CARTESIAN_POINT('Origin',(-0.0866025403784439,-0.4,0.15));
#14357=CARTESIAN_POINT('',(-0.0866025403784439,-0.4,0.15));
#14358=CARTESIAN_POINT('',(-0.173205080756888,-0.4,-2.12115047744981E-17));
#14359=CARTESIAN_POINT('',(-0.0866025403784439,-0.64,0.15));
#14360=CARTESIAN_POINT('',(-0.0866025403784439,-0.4,0.15));
#14361=CARTESIAN_POINT('',(-0.173205080756888,-0.64,-2.12115047744981E-17));
#14362=CARTESIAN_POINT('Origin',(0.0866025403784439,-0.4,0.15));
#14363=CARTESIAN_POINT('',(0.0866025403784439,-0.4,0.15));
#14364=CARTESIAN_POINT('',(-0.0866025403784439,-0.4,0.15));
#14365=CARTESIAN_POINT('',(0.0866025403784439,-0.64,0.15));
#14366=CARTESIAN_POINT('',(0.0866025403784439,-0.4,0.15));
#14367=CARTESIAN_POINT('',(-0.0866025403784439,-0.64,0.15));
#14368=CARTESIAN_POINT('Origin',(0.173205080756888,-0.4,0.));
#14369=CARTESIAN_POINT('',(0.0866025403784439,-0.4,0.15));
#14370=CARTESIAN_POINT('',(0.0866025403784439,-0.64,0.15));
#14371=CARTESIAN_POINT('Origin',(0.,-0.4,-2.77555756156289E-17));
#14372=CARTESIAN_POINT('Origin',(0.,-0.64,-2.77555756156289E-17));
#14373=CARTESIAN_POINT('',(0.,0.,0.));
#14374=CARTESIAN_POINT('',(0.,0.,0.));
#14375=CARTESIAN_POINT('',(0.,0.,0.));
#14376=CARTESIAN_POINT('',(2.40416305603426,2.40416305603426,1.8));
#14377=CARTESIAN_POINT('',(-2.40416305603426,2.40416305603426,1.8));
#14378=CARTESIAN_POINT('',(-2.40416305603426,-2.40416305603426,1.8));
#14379=CARTESIAN_POINT('',(2.40416305603426,-2.40416305603426,1.8));
#14380=CARTESIAN_POINT('',(0.,0.,3.5));
#14381=CARTESIAN_POINT('',(3.4,0.,5.));
#14382=CARTESIAN_POINT('',(0.,3.4,5.));
#14383=CARTESIAN_POINT('',(-3.4,4.163799117101E-16,5.));
#14384=CARTESIAN_POINT('',(-4.44089209850063E-16,-3.4,5.));
#14385=CARTESIAN_POINT('',(0.,0.,0.));
#14386=CARTESIAN_POINT('',(0.,0.,0.));
#14387=CARTESIAN_POINT('',(0.,0.,0.));
#14388=CARTESIAN_POINT('Origin',(0.0721687836487032,0.,-0.125));
#14389=CARTESIAN_POINT('',(0.0721687836487032,0.,-0.125));
#14390=CARTESIAN_POINT('',(0.144337567297406,0.,0.));
#14391=CARTESIAN_POINT('',(0.117710979560879,0.,-0.0461186027918559));
#14392=CARTESIAN_POINT('',(0.0721687836487032,-0.25,-0.125));
#14393=CARTESIAN_POINT('',(0.0721687836487032,0.,-0.125));
#14394=CARTESIAN_POINT('',(0.144337567297406,-0.25,0.));
#14395=CARTESIAN_POINT('',(0.144337567297406,-0.25,0.));
#14396=CARTESIAN_POINT('',(0.144337567297406,0.,0.));
#14397=CARTESIAN_POINT('Origin',(-0.0721687836487032,0.,-0.125));
#14398=CARTESIAN_POINT('',(-0.0721687836487032,0.,-0.125));
#14399=CARTESIAN_POINT('',(0.0739156081756484,0.,-0.125));
#14400=CARTESIAN_POINT('',(-0.0721687836487032,-0.25,-0.125));
#14401=CARTESIAN_POINT('',(-0.0721687836487032,0.,-0.125));
#14402=CARTESIAN_POINT('',(0.0721687836487032,-0.25,-0.125));
#14403=CARTESIAN_POINT('Origin',(-0.144337567297406,0.,-4.16333634234434E-17));
#14404=CARTESIAN_POINT('',(-0.144337567297406,0.,-1.76762539787485E-17));
#14405=CARTESIAN_POINT('',(-0.0987953713852306,0.,-0.0788813972081442));
#14406=CARTESIAN_POINT('',(-0.144337567297406,-0.25,-2.77555756156289E-17));
#14407=CARTESIAN_POINT('',(-0.144337567297406,0.,-1.76762539787485E-17));
#14408=CARTESIAN_POINT('',(-0.0721687836487032,-0.25,-0.125));
#14409=CARTESIAN_POINT('Origin',(-0.0721687836487033,0.,0.125));
#14410=CARTESIAN_POINT('',(-0.0721687836487033,0.,0.125));
#14411=CARTESIAN_POINT('',(-0.0627109795608791,0.,0.141381397208144));
#14412=CARTESIAN_POINT('',(-0.0721687836487033,-0.25,0.125));
#14413=CARTESIAN_POINT('',(-0.0721687836487033,0.,0.125));
#14414=CARTESIAN_POINT('',(-0.144337567297406,-0.25,-1.76762539787485E-17));
#14415=CARTESIAN_POINT('Origin',(0.0721687836487032,0.,0.125));
#14416=CARTESIAN_POINT('',(0.0721687836487032,0.,0.125));
#14417=CARTESIAN_POINT('',(0.146084391824352,0.,0.125));
#14418=CARTESIAN_POINT('',(0.0721687836487032,-0.25,0.125));
#14419=CARTESIAN_POINT('',(0.0721687836487032,0.,0.125));
#14420=CARTESIAN_POINT('',(-0.0721687836487033,-0.25,0.125));
#14421=CARTESIAN_POINT('Origin',(0.144337567297406,0.,0.));
#14422=CARTESIAN_POINT('',(0.153795371385231,0.,-0.0163813972081441));
#14423=CARTESIAN_POINT('',(0.0721687836487032,-0.25,0.125));
#14424=CARTESIAN_POINT('Origin',(0.,-0.25,0.));
#14425=CARTESIAN_POINT('Origin',(0.22,0.,0.));
#14426=CARTESIAN_POINT('',(-0.22,-8.67361737988404E-18,-2.69422295812418E-17));
#14427=CARTESIAN_POINT('Origin',(0.,0.,0.));
#14428=CARTESIAN_POINT('Origin',(0.,-0.015,0.));
#14429=CARTESIAN_POINT('',(-0.24505,-0.02505,-3.00099698131059E-17));
#14430=CARTESIAN_POINT('Origin',(0.,-0.02505,0.));
#14431=CARTESIAN_POINT('',(-0.235,-0.015,-2.87791997799628E-17));
#14432=CARTESIAN_POINT('Origin',(0.,-0.3775,0.));
#14433=CARTESIAN_POINT('',(-0.24505,-0.72995,3.00099698131059E-17));
#14434=CARTESIAN_POINT('Origin',(0.,-0.72995,0.));
#14435=CARTESIAN_POINT('',(-0.24505,-0.3775,-3.00099698131059E-17));
#14436=CARTESIAN_POINT('Origin',(0.,-0.7625,0.));
#14437=CARTESIAN_POINT('',(-0.175,-0.8,-2.14313189850787E-17));
#14438=CARTESIAN_POINT('Origin',(0.,-0.8,0.));
#14439=CARTESIAN_POINT('',(-0.2125,-0.7625,-2.60237444818813E-17));
#14440=CARTESIAN_POINT('Origin',(0.,-0.8,0.));
#14441=CARTESIAN_POINT('',(0.,0.,0.));
#14442=CARTESIAN_POINT('',(0.,0.,0.));
#14443=CARTESIAN_POINT('',(0.,0.,0.));
#14444=CARTESIAN_POINT('',(1.2,0.,6.7));
#14445=CARTESIAN_POINT('',(-0.6,1.03923048454133,6.7));
#14446=CARTESIAN_POINT('',(-0.6,-1.03923048454133,6.7));
#14447=CARTESIAN_POINT('',(0.,2.05,2.4));
#14448=CARTESIAN_POINT('',(0.,0.,0.));
#14449=CARTESIAN_POINT('',(0.,0.,0.));
#14450=CARTESIAN_POINT('Origin',(1.8,13.,0.9));
#14451=CARTESIAN_POINT('',(1.525,13.,1.));
#14452=CARTESIAN_POINT('Origin',(1.8,13.,1.));
#14453=CARTESIAN_POINT('',(1.525,13.,1.4));
#14454=CARTESIAN_POINT('',(1.525,13.,0.9));
#14455=CARTESIAN_POINT('Origin',(1.8,13.,1.4));
#14456=CARTESIAN_POINT('Origin',(-1.8,17.,0.9));
#14457=CARTESIAN_POINT('',(-2.075,17.,1.));
#14458=CARTESIAN_POINT('Origin',(-1.8,17.,1.));
#14459=CARTESIAN_POINT('',(-2.075,17.,1.4));
#14460=CARTESIAN_POINT('',(-2.075,17.,0.9));
#14461=CARTESIAN_POINT('Origin',(-1.8,17.,1.4));
#14462=CARTESIAN_POINT('Origin',(-1.8,13.,0.9));
#14463=CARTESIAN_POINT('',(-2.075,13.,1.));
#14464=CARTESIAN_POINT('Origin',(-1.8,13.,1.));
#14465=CARTESIAN_POINT('',(-2.075,13.,1.4));
#14466=CARTESIAN_POINT('',(-2.075,13.,0.9));
#14467=CARTESIAN_POINT('Origin',(-1.8,13.,1.4));
#14468=CARTESIAN_POINT('Origin',(1.8,17.,0.9));
#14469=CARTESIAN_POINT('',(1.525,17.,1.));
#14470=CARTESIAN_POINT('Origin',(1.8,17.,1.));
#14471=CARTESIAN_POINT('',(1.525,17.,1.4));
#14472=CARTESIAN_POINT('',(1.525,17.,0.9));
#14473=CARTESIAN_POINT('Origin',(1.8,17.,1.4));
#14474=CARTESIAN_POINT('Origin',(0.,13.6,3.5));
#14475=CARTESIAN_POINT('',(-0.5,13.7,3.5));
#14476=CARTESIAN_POINT('Origin',(0.,13.7,3.5));
#14477=CARTESIAN_POINT('',(-0.5,14.1,3.5));
#14478=CARTESIAN_POINT('',(-0.5,13.6,3.5));
#14479=CARTESIAN_POINT('Origin',(0.,14.1,3.5));
#14480=CARTESIAN_POINT('Origin',(0.,13.6,3.5));
#14481=CARTESIAN_POINT('',(-0.5,15.9,3.5));
#14482=CARTESIAN_POINT('Origin',(0.,15.9,3.5));
#14483=CARTESIAN_POINT('',(-0.5,16.3,3.5));
#14484=CARTESIAN_POINT('',(-0.5,13.6,3.5));
#14485=CARTESIAN_POINT('Origin',(0.,16.3,3.5));
#14486=CARTESIAN_POINT('Origin',(-1.8,15.9,1.4));
#14487=CARTESIAN_POINT('',(-1.8,15.9,4.5));
#14488=CARTESIAN_POINT('',(-1.8,15.9,1.4));
#14489=CARTESIAN_POINT('',(-1.8,15.9,4.5));
#14490=CARTESIAN_POINT('',(-1.8,16.3,4.5));
#14491=CARTESIAN_POINT('',(-1.8,15.9,4.5));
#14492=CARTESIAN_POINT('',(-1.8,16.3,1.4));
#14493=CARTESIAN_POINT('',(-1.8,16.3,4.5));
#14494=CARTESIAN_POINT('',(-1.8,15.45,1.4));
#14495=CARTESIAN_POINT('Origin',(1.8,15.9,4.5));
#14496=CARTESIAN_POINT('',(1.8,15.9,1.4));
#14497=CARTESIAN_POINT('',(1.8,15.9,4.5));
#14498=CARTESIAN_POINT('',(1.8,15.9,1.4));
#14499=CARTESIAN_POINT('',(1.8,16.3,1.4));
#14500=CARTESIAN_POINT('',(1.8,15.45,1.4));
#14501=CARTESIAN_POINT('',(1.8,16.3,4.5));
#14502=CARTESIAN_POINT('',(1.8,16.3,1.4));
#14503=CARTESIAN_POINT('',(1.8,15.9,4.5));
#14504=CARTESIAN_POINT('Origin',(-1.8,15.9,4.5));
#14505=CARTESIAN_POINT('',(1.8,15.9,4.5));
#14506=CARTESIAN_POINT('',(1.8,16.3,4.5));
#14507=CARTESIAN_POINT('Origin',(0.,16.3,2.95));
#14508=CARTESIAN_POINT('',(0.,16.3,1.4));
#14509=CARTESIAN_POINT('Origin',(0.,15.9,2.95));
#14510=CARTESIAN_POINT('',(0.,15.9,1.4));
#14511=CARTESIAN_POINT('Origin',(-1.8,13.7,1.4));
#14512=CARTESIAN_POINT('',(-1.8,13.7,4.5));
#14513=CARTESIAN_POINT('',(-1.8,13.7,1.4));
#14514=CARTESIAN_POINT('',(-1.8,13.7,4.5));
#14515=CARTESIAN_POINT('',(-1.8,14.1,4.5));
#14516=CARTESIAN_POINT('',(-1.8,13.7,4.5));
#14517=CARTESIAN_POINT('',(-1.8,14.1,1.4));
#14518=CARTESIAN_POINT('',(-1.8,14.1,4.5));
#14519=CARTESIAN_POINT('',(-1.8,14.35,1.4));
#14520=CARTESIAN_POINT('Origin',(1.8,13.7,4.5));
#14521=CARTESIAN_POINT('',(1.8,13.7,1.4));
#14522=CARTESIAN_POINT('',(1.8,13.7,4.5));
#14523=CARTESIAN_POINT('',(1.8,13.7,1.4));
#14524=CARTESIAN_POINT('',(1.8,14.1,1.4));
#14525=CARTESIAN_POINT('',(1.8,14.35,1.4));
#14526=CARTESIAN_POINT('',(1.8,14.1,4.5));
#14527=CARTESIAN_POINT('',(1.8,14.1,1.4));
#14528=CARTESIAN_POINT('',(1.8,13.7,4.5));
#14529=CARTESIAN_POINT('Origin',(-1.8,13.7,4.5));
#14530=CARTESIAN_POINT('',(1.8,13.7,4.5));
#14531=CARTESIAN_POINT('',(1.8,14.1,4.5));
#14532=CARTESIAN_POINT('Origin',(0.,14.1,2.95));
#14533=CARTESIAN_POINT('',(0.,14.1,1.4));
#14534=CARTESIAN_POINT('Origin',(0.,13.7,2.95));
#14535=CARTESIAN_POINT('',(0.,13.7,1.4));
#14536=CARTESIAN_POINT('Origin',(2.5,17.5,1.));
#14537=CARTESIAN_POINT('',(2.5,17.5,1.));
#14538=CARTESIAN_POINT('',(-2.5,17.5,1.));
#14539=CARTESIAN_POINT('',(2.5,17.5,1.));
#14540=CARTESIAN_POINT('',(-2.5,17.5,1.4));
#14541=CARTESIAN_POINT('',(-2.5,17.5,1.));
#14542=CARTESIAN_POINT('',(2.5,17.5,1.4));
#14543=CARTESIAN_POINT('',(2.5,17.5,1.4));
#14544=CARTESIAN_POINT('',(2.5,17.5,1.));
#14545=CARTESIAN_POINT('Origin',(2.5,12.5,1.));
#14546=CARTESIAN_POINT('',(2.5,12.5,1.));
#14547=CARTESIAN_POINT('',(2.5,12.5,1.));
#14548=CARTESIAN_POINT('',(2.5,12.5,1.4));
#14549=CARTESIAN_POINT('',(2.5,12.5,1.4));
#14550=CARTESIAN_POINT('',(2.5,12.5,1.));
#14551=CARTESIAN_POINT('Origin',(-2.5,12.5,1.));
#14552=CARTESIAN_POINT('',(-2.5,12.5,1.));
#14553=CARTESIAN_POINT('',(-2.5,12.5,1.));
#14554=CARTESIAN_POINT('',(-2.5,12.5,1.4));
#14555=CARTESIAN_POINT('',(-2.5,12.5,1.4));
#14556=CARTESIAN_POINT('',(-2.5,12.5,1.));
#14557=CARTESIAN_POINT('Origin',(-2.5,17.5,1.));
#14558=CARTESIAN_POINT('',(-2.5,17.5,1.));
#14559=CARTESIAN_POINT('',(-2.5,17.5,1.4));
#14560=CARTESIAN_POINT('Origin',(0.,15.,1.4));
#14561=CARTESIAN_POINT('Origin',(0.,15.,1.));
#14562=CARTESIAN_POINT('',(0.,0.,0.));
#14563=CARTESIAN_POINT('Origin',(0.,15.2,3.5));
#14564=CARTESIAN_POINT('',(-0.165,15.2,3.5));
#14565=CARTESIAN_POINT('Origin',(0.,15.2,3.5));
#14566=CARTESIAN_POINT('',(-0.165,16.3,3.5));
#14567=CARTESIAN_POINT('',(-0.165,15.2,3.5));
#14568=CARTESIAN_POINT('Origin',(0.,16.3,3.5));
#14569=CARTESIAN_POINT('Origin',(0.,15.2,3.5));
#14570=CARTESIAN_POINT('Origin',(0.,13.7,3.5));
#14571=CARTESIAN_POINT('',(-0.8,13.7,3.5));
#14572=CARTESIAN_POINT('Origin',(0.,13.7,3.5));
#14573=CARTESIAN_POINT('',(-0.5,13.7,3.5));
#14574=CARTESIAN_POINT('Origin',(0.,13.7,3.5));
#14575=CARTESIAN_POINT('Origin',(0.,13.3,3.5));
#14576=CARTESIAN_POINT('',(-0.8,13.3,3.5));
#14577=CARTESIAN_POINT('',(-0.8,13.3,3.5));
#14578=CARTESIAN_POINT('Origin',(0.,13.3,3.5));
#14579=CARTESIAN_POINT('Origin',(0.,13.3,3.5));
#14580=CARTESIAN_POINT('Origin',(0.,13.7,3.5));
#14581=CARTESIAN_POINT('',(-0.5,16.3,3.5));
#14582=CARTESIAN_POINT('Origin',(0.,16.3,3.5));
#14583=CARTESIAN_POINT('',(-0.5,13.7,3.5));
#14584=CARTESIAN_POINT('Origin',(0.,16.3,3.5));
#14585=CARTESIAN_POINT('',(0.,0.,0.));
#14586=CARTESIAN_POINT('Origin',(0.,14.1,3.5));
#14587=CARTESIAN_POINT('',(-0.505,14.55,3.5));
#14588=CARTESIAN_POINT('Origin',(0.,14.55,3.5));
#14589=CARTESIAN_POINT('',(-0.505,14.1,3.5));
#14590=CARTESIAN_POINT('',(-0.505,14.1,3.5));
#14591=CARTESIAN_POINT('Origin',(0.,14.1,3.5));
#14592=CARTESIAN_POINT('Origin',(0.,14.1,3.5));
#14593=CARTESIAN_POINT('',(-0.7,14.55,3.5));
#14594=CARTESIAN_POINT('Origin',(0.,14.55,3.5));
#14595=CARTESIAN_POINT('',(-0.7,14.1,3.5));
#14596=CARTESIAN_POINT('',(-0.7,14.1,3.5));
#14597=CARTESIAN_POINT('Origin',(0.,14.1,3.5));
#14598=CARTESIAN_POINT('Origin',(0.,14.55,3.5));
#14599=CARTESIAN_POINT('Origin',(0.,14.1,3.5));
#14600=CARTESIAN_POINT('',(0.,0.,0.));
#14601=CARTESIAN_POINT('Origin',(0.,15.45,3.5));
#14602=CARTESIAN_POINT('',(-0.505,15.9,3.5));
#14603=CARTESIAN_POINT('Origin',(0.,15.9,3.5));
#14604=CARTESIAN_POINT('',(-0.505,15.45,3.5));
#14605=CARTESIAN_POINT('',(-0.505,15.45,3.5));
#14606=CARTESIAN_POINT('Origin',(0.,15.45,3.5));
#14607=CARTESIAN_POINT('Origin',(0.,15.45,3.5));
#14608=CARTESIAN_POINT('',(-0.7,15.9,3.5));
#14609=CARTESIAN_POINT('Origin',(0.,15.9,3.5));
#14610=CARTESIAN_POINT('',(-0.7,15.45,3.5));
#14611=CARTESIAN_POINT('',(-0.7,15.45,3.5));
#14612=CARTESIAN_POINT('Origin',(0.,15.45,3.5));
#14613=CARTESIAN_POINT('Origin',(0.,15.9,3.5));
#14614=CARTESIAN_POINT('Origin',(0.,15.45,3.5));
#14615=CARTESIAN_POINT('',(0.,0.,0.));
#14616=CARTESIAN_POINT('Origin',(0.,16.3,3.5));
#14617=CARTESIAN_POINT('',(-0.225,16.5,3.5));
#14618=CARTESIAN_POINT('Origin',(0.,16.5,3.5));
#14619=CARTESIAN_POINT('',(-0.225,16.3,3.5));
#14620=CARTESIAN_POINT('',(-0.225,16.3,3.5));
#14621=CARTESIAN_POINT('Origin',(0.,16.3,3.5));
#14622=CARTESIAN_POINT('Origin',(0.,16.3,3.5));
#14623=CARTESIAN_POINT('',(-0.8,16.5,3.5));
#14624=CARTESIAN_POINT('Origin',(0.,16.5,3.5));
#14625=CARTESIAN_POINT('',(-0.8,16.3,3.5));
#14626=CARTESIAN_POINT('',(-0.8,16.3,3.5));
#14627=CARTESIAN_POINT('Origin',(0.,16.3,3.5));
#14628=CARTESIAN_POINT('Origin',(0.,16.5,3.5));
#14629=CARTESIAN_POINT('Origin',(0.,16.3,3.5));
#14630=CARTESIAN_POINT('',(0.,0.,0.));
#14631=CARTESIAN_POINT('',(0.,0.,0.));
#14632=CARTESIAN_POINT('Origin',(1.8,13.,0.9));
#14633=CARTESIAN_POINT('',(1.525,13.,1.));
#14634=CARTESIAN_POINT('Origin',(1.8,13.,1.));
#14635=CARTESIAN_POINT('',(1.525,13.,1.4));
#14636=CARTESIAN_POINT('',(1.525,13.,0.9));
#14637=CARTESIAN_POINT('Origin',(1.8,13.,1.4));
#14638=CARTESIAN_POINT('Origin',(-1.8,17.,0.9));
#14639=CARTESIAN_POINT('',(-2.075,17.,1.));
#14640=CARTESIAN_POINT('Origin',(-1.8,17.,1.));
#14641=CARTESIAN_POINT('',(-2.075,17.,1.4));
#14642=CARTESIAN_POINT('',(-2.075,17.,0.9));
#14643=CARTESIAN_POINT('Origin',(-1.8,17.,1.4));
#14644=CARTESIAN_POINT('Origin',(-1.8,13.,0.9));
#14645=CARTESIAN_POINT('',(-2.075,13.,1.));
#14646=CARTESIAN_POINT('Origin',(-1.8,13.,1.));
#14647=CARTESIAN_POINT('',(-2.075,13.,1.4));
#14648=CARTESIAN_POINT('',(-2.075,13.,0.9));
#14649=CARTESIAN_POINT('Origin',(-1.8,13.,1.4));
#14650=CARTESIAN_POINT('Origin',(1.8,17.,0.9));
#14651=CARTESIAN_POINT('',(1.525,17.,1.));
#14652=CARTESIAN_POINT('Origin',(1.8,17.,1.));
#14653=CARTESIAN_POINT('',(1.525,17.,1.4));
#14654=CARTESIAN_POINT('',(1.525,17.,0.9));
#14655=CARTESIAN_POINT('Origin',(1.8,17.,1.4));
#14656=CARTESIAN_POINT('Origin',(0.,13.6,3.5));
#14657=CARTESIAN_POINT('',(-0.5,13.7,3.5));
#14658=CARTESIAN_POINT('Origin',(0.,13.7,3.5));
#14659=CARTESIAN_POINT('',(-0.5,14.1,3.5));
#14660=CARTESIAN_POINT('',(-0.5,13.6,3.5));
#14661=CARTESIAN_POINT('Origin',(0.,14.1,3.5));
#14662=CARTESIAN_POINT('Origin',(0.,13.6,3.5));
#14663=CARTESIAN_POINT('',(-0.5,15.9,3.5));
#14664=CARTESIAN_POINT('Origin',(0.,15.9,3.5));
#14665=CARTESIAN_POINT('',(-0.5,16.3,3.5));
#14666=CARTESIAN_POINT('',(-0.5,13.6,3.5));
#14667=CARTESIAN_POINT('Origin',(0.,16.3,3.5));
#14668=CARTESIAN_POINT('Origin',(-1.8,15.9,1.4));
#14669=CARTESIAN_POINT('',(-1.8,15.9,4.5));
#14670=CARTESIAN_POINT('',(-1.8,15.9,1.4));
#14671=CARTESIAN_POINT('',(-1.8,15.9,4.5));
#14672=CARTESIAN_POINT('',(-1.8,16.3,4.5));
#14673=CARTESIAN_POINT('',(-1.8,15.9,4.5));
#14674=CARTESIAN_POINT('',(-1.8,16.3,1.4));
#14675=CARTESIAN_POINT('',(-1.8,16.3,4.5));
#14676=CARTESIAN_POINT('',(-1.8,15.45,1.4));
#14677=CARTESIAN_POINT('Origin',(1.8,15.9,4.5));
#14678=CARTESIAN_POINT('',(1.8,15.9,1.4));
#14679=CARTESIAN_POINT('',(1.8,15.9,4.5));
#14680=CARTESIAN_POINT('',(1.8,15.9,1.4));
#14681=CARTESIAN_POINT('',(1.8,16.3,1.4));
#14682=CARTESIAN_POINT('',(1.8,15.45,1.4));
#14683=CARTESIAN_POINT('',(1.8,16.3,4.5));
#14684=CARTESIAN_POINT('',(1.8,16.3,1.4));
#14685=CARTESIAN_POINT('',(1.8,15.9,4.5));
#14686=CARTESIAN_POINT('Origin',(-1.8,15.9,4.5));
#14687=CARTESIAN_POINT('',(1.8,15.9,4.5));
#14688=CARTESIAN_POINT('',(1.8,16.3,4.5));
#14689=CARTESIAN_POINT('Origin',(0.,16.3,2.95));
#14690=CARTESIAN_POINT('',(0.,16.3,1.4));
#14691=CARTESIAN_POINT('Origin',(0.,15.9,2.95));
#14692=CARTESIAN_POINT('',(0.,15.9,1.4));
#14693=CARTESIAN_POINT('Origin',(-1.8,13.7,1.4));
#14694=CARTESIAN_POINT('',(-1.8,13.7,4.5));
#14695=CARTESIAN_POINT('',(-1.8,13.7,1.4));
#14696=CARTESIAN_POINT('',(-1.8,13.7,4.5));
#14697=CARTESIAN_POINT('',(-1.8,14.1,4.5));
#14698=CARTESIAN_POINT('',(-1.8,13.7,4.5));
#14699=CARTESIAN_POINT('',(-1.8,14.1,1.4));
#14700=CARTESIAN_POINT('',(-1.8,14.1,4.5));
#14701=CARTESIAN_POINT('',(-1.8,14.35,1.4));
#14702=CARTESIAN_POINT('Origin',(1.8,13.7,4.5));
#14703=CARTESIAN_POINT('',(1.8,13.7,1.4));
#14704=CARTESIAN_POINT('',(1.8,13.7,4.5));
#14705=CARTESIAN_POINT('',(1.8,13.7,1.4));
#14706=CARTESIAN_POINT('',(1.8,14.1,1.4));
#14707=CARTESIAN_POINT('',(1.8,14.35,1.4));
#14708=CARTESIAN_POINT('',(1.8,14.1,4.5));
#14709=CARTESIAN_POINT('',(1.8,14.1,1.4));
#14710=CARTESIAN_POINT('',(1.8,13.7,4.5));
#14711=CARTESIAN_POINT('Origin',(-1.8,13.7,4.5));
#14712=CARTESIAN_POINT('',(1.8,13.7,4.5));
#14713=CARTESIAN_POINT('',(1.8,14.1,4.5));
#14714=CARTESIAN_POINT('Origin',(0.,14.1,2.95));
#14715=CARTESIAN_POINT('',(0.,14.1,1.4));
#14716=CARTESIAN_POINT('Origin',(0.,13.7,2.95));
#14717=CARTESIAN_POINT('',(0.,13.7,1.4));
#14718=CARTESIAN_POINT('Origin',(2.5,17.5,1.));
#14719=CARTESIAN_POINT('',(2.5,17.5,1.));
#14720=CARTESIAN_POINT('',(-2.5,17.5,1.));
#14721=CARTESIAN_POINT('',(2.5,17.5,1.));
#14722=CARTESIAN_POINT('',(-2.5,17.5,1.4));
#14723=CARTESIAN_POINT('',(-2.5,17.5,1.));
#14724=CARTESIAN_POINT('',(2.5,17.5,1.4));
#14725=CARTESIAN_POINT('',(2.5,17.5,1.4));
#14726=CARTESIAN_POINT('',(2.5,17.5,1.));
#14727=CARTESIAN_POINT('Origin',(2.5,12.5,1.));
#14728=CARTESIAN_POINT('',(2.5,12.5,1.));
#14729=CARTESIAN_POINT('',(2.5,12.5,1.));
#14730=CARTESIAN_POINT('',(2.5,12.5,1.4));
#14731=CARTESIAN_POINT('',(2.5,12.5,1.4));
#14732=CARTESIAN_POINT('',(2.5,12.5,1.));
#14733=CARTESIAN_POINT('Origin',(-2.5,12.5,1.));
#14734=CARTESIAN_POINT('',(-2.5,12.5,1.));
#14735=CARTESIAN_POINT('',(-2.5,12.5,1.));
#14736=CARTESIAN_POINT('',(-2.5,12.5,1.4));
#14737=CARTESIAN_POINT('',(-2.5,12.5,1.4));
#14738=CARTESIAN_POINT('',(-2.5,12.5,1.));
#14739=CARTESIAN_POINT('Origin',(-2.5,17.5,1.));
#14740=CARTESIAN_POINT('',(-2.5,17.5,1.));
#14741=CARTESIAN_POINT('',(-2.5,17.5,1.4));
#14742=CARTESIAN_POINT('Origin',(0.,15.,1.4));
#14743=CARTESIAN_POINT('Origin',(0.,15.,1.));
#14744=CARTESIAN_POINT('',(0.,0.,0.));
#14745=CARTESIAN_POINT('Origin',(0.,15.2,3.5));
#14746=CARTESIAN_POINT('',(-0.165,15.2,3.5));
#14747=CARTESIAN_POINT('Origin',(0.,15.2,3.5));
#14748=CARTESIAN_POINT('',(-0.165,16.3,3.5));
#14749=CARTESIAN_POINT('',(-0.165,15.2,3.5));
#14750=CARTESIAN_POINT('Origin',(0.,16.3,3.5));
#14751=CARTESIAN_POINT('Origin',(0.,15.2,3.5));
#14752=CARTESIAN_POINT('Origin',(0.,13.7,3.5));
#14753=CARTESIAN_POINT('',(-0.8,13.7,3.5));
#14754=CARTESIAN_POINT('Origin',(0.,13.7,3.5));
#14755=CARTESIAN_POINT('',(-0.5,13.7,3.5));
#14756=CARTESIAN_POINT('Origin',(0.,13.7,3.5));
#14757=CARTESIAN_POINT('Origin',(0.,13.3,3.5));
#14758=CARTESIAN_POINT('',(-0.8,13.3,3.5));
#14759=CARTESIAN_POINT('',(-0.8,13.3,3.5));
#14760=CARTESIAN_POINT('Origin',(0.,13.3,3.5));
#14761=CARTESIAN_POINT('Origin',(0.,13.3,3.5));
#14762=CARTESIAN_POINT('Origin',(0.,13.7,3.5));
#14763=CARTESIAN_POINT('',(-0.5,16.3,3.5));
#14764=CARTESIAN_POINT('Origin',(0.,16.3,3.5));
#14765=CARTESIAN_POINT('',(-0.5,13.7,3.5));
#14766=CARTESIAN_POINT('Origin',(0.,16.3,3.5));
#14767=CARTESIAN_POINT('',(0.,0.,0.));
#14768=CARTESIAN_POINT('Origin',(0.,14.1,3.5));
#14769=CARTESIAN_POINT('',(-0.505,14.55,3.5));
#14770=CARTESIAN_POINT('Origin',(0.,14.55,3.5));
#14771=CARTESIAN_POINT('',(-0.505,14.1,3.5));
#14772=CARTESIAN_POINT('',(-0.505,14.1,3.5));
#14773=CARTESIAN_POINT('Origin',(0.,14.1,3.5));
#14774=CARTESIAN_POINT('Origin',(0.,14.1,3.5));
#14775=CARTESIAN_POINT('',(-0.7,14.55,3.5));
#14776=CARTESIAN_POINT('Origin',(0.,14.55,3.5));
#14777=CARTESIAN_POINT('',(-0.7,14.1,3.5));
#14778=CARTESIAN_POINT('',(-0.7,14.1,3.5));
#14779=CARTESIAN_POINT('Origin',(0.,14.1,3.5));
#14780=CARTESIAN_POINT('Origin',(0.,14.55,3.5));
#14781=CARTESIAN_POINT('Origin',(0.,14.1,3.5));
#14782=CARTESIAN_POINT('',(0.,0.,0.));
#14783=CARTESIAN_POINT('Origin',(0.,15.45,3.5));
#14784=CARTESIAN_POINT('',(-0.505,15.9,3.5));
#14785=CARTESIAN_POINT('Origin',(0.,15.9,3.5));
#14786=CARTESIAN_POINT('',(-0.505,15.45,3.5));
#14787=CARTESIAN_POINT('',(-0.505,15.45,3.5));
#14788=CARTESIAN_POINT('Origin',(0.,15.45,3.5));
#14789=CARTESIAN_POINT('Origin',(0.,15.45,3.5));
#14790=CARTESIAN_POINT('',(-0.7,15.9,3.5));
#14791=CARTESIAN_POINT('Origin',(0.,15.9,3.5));
#14792=CARTESIAN_POINT('',(-0.7,15.45,3.5));
#14793=CARTESIAN_POINT('',(-0.7,15.45,3.5));
#14794=CARTESIAN_POINT('Origin',(0.,15.45,3.5));
#14795=CARTESIAN_POINT('Origin',(0.,15.9,3.5));
#14796=CARTESIAN_POINT('Origin',(0.,15.45,3.5));
#14797=CARTESIAN_POINT('',(0.,0.,0.));
#14798=CARTESIAN_POINT('Origin',(0.,16.3,3.5));
#14799=CARTESIAN_POINT('',(-0.225,16.5,3.5));
#14800=CARTESIAN_POINT('Origin',(0.,16.5,3.5));
#14801=CARTESIAN_POINT('',(-0.225,16.3,3.5));
#14802=CARTESIAN_POINT('',(-0.225,16.3,3.5));
#14803=CARTESIAN_POINT('Origin',(0.,16.3,3.5));
#14804=CARTESIAN_POINT('Origin',(0.,16.3,3.5));
#14805=CARTESIAN_POINT('',(-0.8,16.5,3.5));
#14806=CARTESIAN_POINT('Origin',(0.,16.5,3.5));
#14807=CARTESIAN_POINT('',(-0.8,16.3,3.5));
#14808=CARTESIAN_POINT('',(-0.8,16.3,3.5));
#14809=CARTESIAN_POINT('Origin',(0.,16.3,3.5));
#14810=CARTESIAN_POINT('Origin',(0.,16.5,3.5));
#14811=CARTESIAN_POINT('Origin',(0.,16.3,3.5));
#14812=CARTESIAN_POINT('',(0.,0.,0.));
#14813=CARTESIAN_POINT('',(0.,0.,0.));
#14814=CARTESIAN_POINT('Origin',(1.8,13.,0.9));
#14815=CARTESIAN_POINT('',(1.525,13.,1.));
#14816=CARTESIAN_POINT('Origin',(1.8,13.,1.));
#14817=CARTESIAN_POINT('',(1.525,13.,1.4));
#14818=CARTESIAN_POINT('',(1.525,13.,0.9));
#14819=CARTESIAN_POINT('Origin',(1.8,13.,1.4));
#14820=CARTESIAN_POINT('Origin',(-1.8,17.,0.9));
#14821=CARTESIAN_POINT('',(-2.075,17.,1.));
#14822=CARTESIAN_POINT('Origin',(-1.8,17.,1.));
#14823=CARTESIAN_POINT('',(-2.075,17.,1.4));
#14824=CARTESIAN_POINT('',(-2.075,17.,0.9));
#14825=CARTESIAN_POINT('Origin',(-1.8,17.,1.4));
#14826=CARTESIAN_POINT('Origin',(-1.8,13.,0.9));
#14827=CARTESIAN_POINT('',(-2.075,13.,1.));
#14828=CARTESIAN_POINT('Origin',(-1.8,13.,1.));
#14829=CARTESIAN_POINT('',(-2.075,13.,1.4));
#14830=CARTESIAN_POINT('',(-2.075,13.,0.9));
#14831=CARTESIAN_POINT('Origin',(-1.8,13.,1.4));
#14832=CARTESIAN_POINT('Origin',(1.8,17.,0.9));
#14833=CARTESIAN_POINT('',(1.525,17.,1.));
#14834=CARTESIAN_POINT('Origin',(1.8,17.,1.));
#14835=CARTESIAN_POINT('',(1.525,17.,1.4));
#14836=CARTESIAN_POINT('',(1.525,17.,0.9));
#14837=CARTESIAN_POINT('Origin',(1.8,17.,1.4));
#14838=CARTESIAN_POINT('Origin',(0.,13.6,3.5));
#14839=CARTESIAN_POINT('',(-0.5,13.7,3.5));
#14840=CARTESIAN_POINT('Origin',(0.,13.7,3.5));
#14841=CARTESIAN_POINT('',(-0.5,14.1,3.5));
#14842=CARTESIAN_POINT('',(-0.5,13.6,3.5));
#14843=CARTESIAN_POINT('Origin',(0.,14.1,3.5));
#14844=CARTESIAN_POINT('Origin',(0.,13.6,3.5));
#14845=CARTESIAN_POINT('',(-0.5,15.9,3.5));
#14846=CARTESIAN_POINT('Origin',(0.,15.9,3.5));
#14847=CARTESIAN_POINT('',(-0.5,16.3,3.5));
#14848=CARTESIAN_POINT('',(-0.5,13.6,3.5));
#14849=CARTESIAN_POINT('Origin',(0.,16.3,3.5));
#14850=CARTESIAN_POINT('Origin',(-1.8,15.9,1.4));
#14851=CARTESIAN_POINT('',(-1.8,15.9,4.5));
#14852=CARTESIAN_POINT('',(-1.8,15.9,1.4));
#14853=CARTESIAN_POINT('',(-1.8,15.9,4.5));
#14854=CARTESIAN_POINT('',(-1.8,16.3,4.5));
#14855=CARTESIAN_POINT('',(-1.8,15.9,4.5));
#14856=CARTESIAN_POINT('',(-1.8,16.3,1.4));
#14857=CARTESIAN_POINT('',(-1.8,16.3,4.5));
#14858=CARTESIAN_POINT('',(-1.8,15.45,1.4));
#14859=CARTESIAN_POINT('Origin',(1.8,15.9,4.5));
#14860=CARTESIAN_POINT('',(1.8,15.9,1.4));
#14861=CARTESIAN_POINT('',(1.8,15.9,4.5));
#14862=CARTESIAN_POINT('',(1.8,15.9,1.4));
#14863=CARTESIAN_POINT('',(1.8,16.3,1.4));
#14864=CARTESIAN_POINT('',(1.8,15.45,1.4));
#14865=CARTESIAN_POINT('',(1.8,16.3,4.5));
#14866=CARTESIAN_POINT('',(1.8,16.3,1.4));
#14867=CARTESIAN_POINT('',(1.8,15.9,4.5));
#14868=CARTESIAN_POINT('Origin',(-1.8,15.9,4.5));
#14869=CARTESIAN_POINT('',(1.8,15.9,4.5));
#14870=CARTESIAN_POINT('',(1.8,16.3,4.5));
#14871=CARTESIAN_POINT('Origin',(0.,16.3,2.95));
#14872=CARTESIAN_POINT('',(0.,16.3,1.4));
#14873=CARTESIAN_POINT('Origin',(0.,15.9,2.95));
#14874=CARTESIAN_POINT('',(0.,15.9,1.4));
#14875=CARTESIAN_POINT('Origin',(-1.8,13.7,1.4));
#14876=CARTESIAN_POINT('',(-1.8,13.7,4.5));
#14877=CARTESIAN_POINT('',(-1.8,13.7,1.4));
#14878=CARTESIAN_POINT('',(-1.8,13.7,4.5));
#14879=CARTESIAN_POINT('',(-1.8,14.1,4.5));
#14880=CARTESIAN_POINT('',(-1.8,13.7,4.5));
#14881=CARTESIAN_POINT('',(-1.8,14.1,1.4));
#14882=CARTESIAN_POINT('',(-1.8,14.1,4.5));
#14883=CARTESIAN_POINT('',(-1.8,14.35,1.4));
#14884=CARTESIAN_POINT('Origin',(1.8,13.7,4.5));
#14885=CARTESIAN_POINT('',(1.8,13.7,1.4));
#14886=CARTESIAN_POINT('',(1.8,13.7,4.5));
#14887=CARTESIAN_POINT('',(1.8,13.7,1.4));
#14888=CARTESIAN_POINT('',(1.8,14.1,1.4));
#14889=CARTESIAN_POINT('',(1.8,14.35,1.4));
#14890=CARTESIAN_POINT('',(1.8,14.1,4.5));
#14891=CARTESIAN_POINT('',(1.8,14.1,1.4));
#14892=CARTESIAN_POINT('',(1.8,13.7,4.5));
#14893=CARTESIAN_POINT('Origin',(-1.8,13.7,4.5));
#14894=CARTESIAN_POINT('',(1.8,13.7,4.5));
#14895=CARTESIAN_POINT('',(1.8,14.1,4.5));
#14896=CARTESIAN_POINT('Origin',(0.,14.1,2.95));
#14897=CARTESIAN_POINT('',(0.,14.1,1.4));
#14898=CARTESIAN_POINT('Origin',(0.,13.7,2.95));
#14899=CARTESIAN_POINT('',(0.,13.7,1.4));
#14900=CARTESIAN_POINT('Origin',(2.5,17.5,1.));
#14901=CARTESIAN_POINT('',(2.5,17.5,1.));
#14902=CARTESIAN_POINT('',(-2.5,17.5,1.));
#14903=CARTESIAN_POINT('',(2.5,17.5,1.));
#14904=CARTESIAN_POINT('',(-2.5,17.5,1.4));
#14905=CARTESIAN_POINT('',(-2.5,17.5,1.));
#14906=CARTESIAN_POINT('',(2.5,17.5,1.4));
#14907=CARTESIAN_POINT('',(2.5,17.5,1.4));
#14908=CARTESIAN_POINT('',(2.5,17.5,1.));
#14909=CARTESIAN_POINT('Origin',(2.5,12.5,1.));
#14910=CARTESIAN_POINT('',(2.5,12.5,1.));
#14911=CARTESIAN_POINT('',(2.5,12.5,1.));
#14912=CARTESIAN_POINT('',(2.5,12.5,1.4));
#14913=CARTESIAN_POINT('',(2.5,12.5,1.4));
#14914=CARTESIAN_POINT('',(2.5,12.5,1.));
#14915=CARTESIAN_POINT('Origin',(-2.5,12.5,1.));
#14916=CARTESIAN_POINT('',(-2.5,12.5,1.));
#14917=CARTESIAN_POINT('',(-2.5,12.5,1.));
#14918=CARTESIAN_POINT('',(-2.5,12.5,1.4));
#14919=CARTESIAN_POINT('',(-2.5,12.5,1.4));
#14920=CARTESIAN_POINT('',(-2.5,12.5,1.));
#14921=CARTESIAN_POINT('Origin',(-2.5,17.5,1.));
#14922=CARTESIAN_POINT('',(-2.5,17.5,1.));
#14923=CARTESIAN_POINT('',(-2.5,17.5,1.4));
#14924=CARTESIAN_POINT('Origin',(0.,15.,1.4));
#14925=CARTESIAN_POINT('Origin',(0.,15.,1.));
#14926=CARTESIAN_POINT('',(0.,0.,0.));
#14927=CARTESIAN_POINT('Origin',(0.,15.2,3.5));
#14928=CARTESIAN_POINT('',(-0.165,15.2,3.5));
#14929=CARTESIAN_POINT('Origin',(0.,15.2,3.5));
#14930=CARTESIAN_POINT('',(-0.165,16.3,3.5));
#14931=CARTESIAN_POINT('',(-0.165,15.2,3.5));
#14932=CARTESIAN_POINT('Origin',(0.,16.3,3.5));
#14933=CARTESIAN_POINT('Origin',(0.,15.2,3.5));
#14934=CARTESIAN_POINT('Origin',(0.,13.7,3.5));
#14935=CARTESIAN_POINT('',(-0.8,13.7,3.5));
#14936=CARTESIAN_POINT('Origin',(0.,13.7,3.5));
#14937=CARTESIAN_POINT('',(-0.5,13.7,3.5));
#14938=CARTESIAN_POINT('Origin',(0.,13.7,3.5));
#14939=CARTESIAN_POINT('Origin',(0.,13.3,3.5));
#14940=CARTESIAN_POINT('',(-0.8,13.3,3.5));
#14941=CARTESIAN_POINT('',(-0.8,13.3,3.5));
#14942=CARTESIAN_POINT('Origin',(0.,13.3,3.5));
#14943=CARTESIAN_POINT('Origin',(0.,13.3,3.5));
#14944=CARTESIAN_POINT('Origin',(0.,13.7,3.5));
#14945=CARTESIAN_POINT('',(-0.5,16.3,3.5));
#14946=CARTESIAN_POINT('Origin',(0.,16.3,3.5));
#14947=CARTESIAN_POINT('',(-0.5,13.7,3.5));
#14948=CARTESIAN_POINT('Origin',(0.,16.3,3.5));
#14949=CARTESIAN_POINT('',(0.,0.,0.));
#14950=CARTESIAN_POINT('Origin',(0.,14.1,3.5));
#14951=CARTESIAN_POINT('',(-0.505,14.55,3.5));
#14952=CARTESIAN_POINT('Origin',(0.,14.55,3.5));
#14953=CARTESIAN_POINT('',(-0.505,14.1,3.5));
#14954=CARTESIAN_POINT('',(-0.505,14.1,3.5));
#14955=CARTESIAN_POINT('Origin',(0.,14.1,3.5));
#14956=CARTESIAN_POINT('Origin',(0.,14.1,3.5));
#14957=CARTESIAN_POINT('',(-0.7,14.55,3.5));
#14958=CARTESIAN_POINT('Origin',(0.,14.55,3.5));
#14959=CARTESIAN_POINT('',(-0.7,14.1,3.5));
#14960=CARTESIAN_POINT('',(-0.7,14.1,3.5));
#14961=CARTESIAN_POINT('Origin',(0.,14.1,3.5));
#14962=CARTESIAN_POINT('Origin',(0.,14.55,3.5));
#14963=CARTESIAN_POINT('Origin',(0.,14.1,3.5));
#14964=CARTESIAN_POINT('',(0.,0.,0.));
#14965=CARTESIAN_POINT('Origin',(0.,15.45,3.5));
#14966=CARTESIAN_POINT('',(-0.505,15.9,3.5));
#14967=CARTESIAN_POINT('Origin',(0.,15.9,3.5));
#14968=CARTESIAN_POINT('',(-0.505,15.45,3.5));
#14969=CARTESIAN_POINT('',(-0.505,15.45,3.5));
#14970=CARTESIAN_POINT('Origin',(0.,15.45,3.5));
#14971=CARTESIAN_POINT('Origin',(0.,15.45,3.5));
#14972=CARTESIAN_POINT('',(-0.7,15.9,3.5));
#14973=CARTESIAN_POINT('Origin',(0.,15.9,3.5));
#14974=CARTESIAN_POINT('',(-0.7,15.45,3.5));
#14975=CARTESIAN_POINT('',(-0.7,15.45,3.5));
#14976=CARTESIAN_POINT('Origin',(0.,15.45,3.5));
#14977=CARTESIAN_POINT('Origin',(0.,15.9,3.5));
#14978=CARTESIAN_POINT('Origin',(0.,15.45,3.5));
#14979=CARTESIAN_POINT('',(0.,0.,0.));
#14980=CARTESIAN_POINT('Origin',(0.,16.3,3.5));
#14981=CARTESIAN_POINT('',(-0.225,16.5,3.5));
#14982=CARTESIAN_POINT('Origin',(0.,16.5,3.5));
#14983=CARTESIAN_POINT('',(-0.225,16.3,3.5));
#14984=CARTESIAN_POINT('',(-0.225,16.3,3.5));
#14985=CARTESIAN_POINT('Origin',(0.,16.3,3.5));
#14986=CARTESIAN_POINT('Origin',(0.,16.3,3.5));
#14987=CARTESIAN_POINT('',(-0.8,16.5,3.5));
#14988=CARTESIAN_POINT('Origin',(0.,16.5,3.5));
#14989=CARTESIAN_POINT('',(-0.8,16.3,3.5));
#14990=CARTESIAN_POINT('',(-0.8,16.3,3.5));
#14991=CARTESIAN_POINT('Origin',(0.,16.3,3.5));
#14992=CARTESIAN_POINT('Origin',(0.,16.5,3.5));
#14993=CARTESIAN_POINT('Origin',(0.,16.3,3.5));
#14994=CARTESIAN_POINT('',(0.,0.,0.));
#14995=CARTESIAN_POINT('',(0.,0.,0.));
#14996=CARTESIAN_POINT('Origin',(1.8,13.,0.9));
#14997=CARTESIAN_POINT('',(1.525,13.,1.));
#14998=CARTESIAN_POINT('Origin',(1.8,13.,1.));
#14999=CARTESIAN_POINT('',(1.525,13.,1.4));
#15000=CARTESIAN_POINT('',(1.525,13.,0.9));
#15001=CARTESIAN_POINT('Origin',(1.8,13.,1.4));
#15002=CARTESIAN_POINT('Origin',(-1.8,17.,0.9));
#15003=CARTESIAN_POINT('',(-2.075,17.,1.));
#15004=CARTESIAN_POINT('Origin',(-1.8,17.,1.));
#15005=CARTESIAN_POINT('',(-2.075,17.,1.4));
#15006=CARTESIAN_POINT('',(-2.075,17.,0.9));
#15007=CARTESIAN_POINT('Origin',(-1.8,17.,1.4));
#15008=CARTESIAN_POINT('Origin',(-1.8,13.,0.9));
#15009=CARTESIAN_POINT('',(-2.075,13.,1.));
#15010=CARTESIAN_POINT('Origin',(-1.8,13.,1.));
#15011=CARTESIAN_POINT('',(-2.075,13.,1.4));
#15012=CARTESIAN_POINT('',(-2.075,13.,0.9));
#15013=CARTESIAN_POINT('Origin',(-1.8,13.,1.4));
#15014=CARTESIAN_POINT('Origin',(1.8,17.,0.9));
#15015=CARTESIAN_POINT('',(1.525,17.,1.));
#15016=CARTESIAN_POINT('Origin',(1.8,17.,1.));
#15017=CARTESIAN_POINT('',(1.525,17.,1.4));
#15018=CARTESIAN_POINT('',(1.525,17.,0.9));
#15019=CARTESIAN_POINT('Origin',(1.8,17.,1.4));
#15020=CARTESIAN_POINT('Origin',(0.,13.6,3.5));
#15021=CARTESIAN_POINT('',(-0.5,13.7,3.5));
#15022=CARTESIAN_POINT('Origin',(0.,13.7,3.5));
#15023=CARTESIAN_POINT('',(-0.5,14.1,3.5));
#15024=CARTESIAN_POINT('',(-0.5,13.6,3.5));
#15025=CARTESIAN_POINT('Origin',(0.,14.1,3.5));
#15026=CARTESIAN_POINT('Origin',(0.,13.6,3.5));
#15027=CARTESIAN_POINT('',(-0.5,15.9,3.5));
#15028=CARTESIAN_POINT('Origin',(0.,15.9,3.5));
#15029=CARTESIAN_POINT('',(-0.5,16.3,3.5));
#15030=CARTESIAN_POINT('',(-0.5,13.6,3.5));
#15031=CARTESIAN_POINT('Origin',(0.,16.3,3.5));
#15032=CARTESIAN_POINT('Origin',(-1.8,15.9,1.4));
#15033=CARTESIAN_POINT('',(-1.8,15.9,4.5));
#15034=CARTESIAN_POINT('',(-1.8,15.9,1.4));
#15035=CARTESIAN_POINT('',(-1.8,15.9,4.5));
#15036=CARTESIAN_POINT('',(-1.8,16.3,4.5));
#15037=CARTESIAN_POINT('',(-1.8,15.9,4.5));
#15038=CARTESIAN_POINT('',(-1.8,16.3,1.4));
#15039=CARTESIAN_POINT('',(-1.8,16.3,4.5));
#15040=CARTESIAN_POINT('',(-1.8,15.45,1.4));
#15041=CARTESIAN_POINT('Origin',(1.8,15.9,4.5));
#15042=CARTESIAN_POINT('',(1.8,15.9,1.4));
#15043=CARTESIAN_POINT('',(1.8,15.9,4.5));
#15044=CARTESIAN_POINT('',(1.8,15.9,1.4));
#15045=CARTESIAN_POINT('',(1.8,16.3,1.4));
#15046=CARTESIAN_POINT('',(1.8,15.45,1.4));
#15047=CARTESIAN_POINT('',(1.8,16.3,4.5));
#15048=CARTESIAN_POINT('',(1.8,16.3,1.4));
#15049=CARTESIAN_POINT('',(1.8,15.9,4.5));
#15050=CARTESIAN_POINT('Origin',(-1.8,15.9,4.5));
#15051=CARTESIAN_POINT('',(1.8,15.9,4.5));
#15052=CARTESIAN_POINT('',(1.8,16.3,4.5));
#15053=CARTESIAN_POINT('Origin',(0.,16.3,2.95));
#15054=CARTESIAN_POINT('',(0.,16.3,1.4));
#15055=CARTESIAN_POINT('Origin',(0.,15.9,2.95));
#15056=CARTESIAN_POINT('',(0.,15.9,1.4));
#15057=CARTESIAN_POINT('Origin',(-1.8,13.7,1.4));
#15058=CARTESIAN_POINT('',(-1.8,13.7,4.5));
#15059=CARTESIAN_POINT('',(-1.8,13.7,1.4));
#15060=CARTESIAN_POINT('',(-1.8,13.7,4.5));
#15061=CARTESIAN_POINT('',(-1.8,14.1,4.5));
#15062=CARTESIAN_POINT('',(-1.8,13.7,4.5));
#15063=CARTESIAN_POINT('',(-1.8,14.1,1.4));
#15064=CARTESIAN_POINT('',(-1.8,14.1,4.5));
#15065=CARTESIAN_POINT('',(-1.8,14.35,1.4));
#15066=CARTESIAN_POINT('Origin',(1.8,13.7,4.5));
#15067=CARTESIAN_POINT('',(1.8,13.7,1.4));
#15068=CARTESIAN_POINT('',(1.8,13.7,4.5));
#15069=CARTESIAN_POINT('',(1.8,13.7,1.4));
#15070=CARTESIAN_POINT('',(1.8,14.1,1.4));
#15071=CARTESIAN_POINT('',(1.8,14.35,1.4));
#15072=CARTESIAN_POINT('',(1.8,14.1,4.5));
#15073=CARTESIAN_POINT('',(1.8,14.1,1.4));
#15074=CARTESIAN_POINT('',(1.8,13.7,4.5));
#15075=CARTESIAN_POINT('Origin',(-1.8,13.7,4.5));
#15076=CARTESIAN_POINT('',(1.8,13.7,4.5));
#15077=CARTESIAN_POINT('',(1.8,14.1,4.5));
#15078=CARTESIAN_POINT('Origin',(0.,14.1,2.95));
#15079=CARTESIAN_POINT('',(0.,14.1,1.4));
#15080=CARTESIAN_POINT('Origin',(0.,13.7,2.95));
#15081=CARTESIAN_POINT('',(0.,13.7,1.4));
#15082=CARTESIAN_POINT('Origin',(2.5,17.5,1.));
#15083=CARTESIAN_POINT('',(2.5,17.5,1.));
#15084=CARTESIAN_POINT('',(-2.5,17.5,1.));
#15085=CARTESIAN_POINT('',(2.5,17.5,1.));
#15086=CARTESIAN_POINT('',(-2.5,17.5,1.4));
#15087=CARTESIAN_POINT('',(-2.5,17.5,1.));
#15088=CARTESIAN_POINT('',(2.5,17.5,1.4));
#15089=CARTESIAN_POINT('',(2.5,17.5,1.4));
#15090=CARTESIAN_POINT('',(2.5,17.5,1.));
#15091=CARTESIAN_POINT('Origin',(2.5,12.5,1.));
#15092=CARTESIAN_POINT('',(2.5,12.5,1.));
#15093=CARTESIAN_POINT('',(2.5,12.5,1.));
#15094=CARTESIAN_POINT('',(2.5,12.5,1.4));
#15095=CARTESIAN_POINT('',(2.5,12.5,1.4));
#15096=CARTESIAN_POINT('',(2.5,12.5,1.));
#15097=CARTESIAN_POINT('Origin',(-2.5,12.5,1.));
#15098=CARTESIAN_POINT('',(-2.5,12.5,1.));
#15099=CARTESIAN_POINT('',(-2.5,12.5,1.));
#15100=CARTESIAN_POINT('',(-2.5,12.5,1.4));
#15101=CARTESIAN_POINT('',(-2.5,12.5,1.4));
#15102=CARTESIAN_POINT('',(-2.5,12.5,1.));
#15103=CARTESIAN_POINT('Origin',(-2.5,17.5,1.));
#15104=CARTESIAN_POINT('',(-2.5,17.5,1.));
#15105=CARTESIAN_POINT('',(-2.5,17.5,1.4));
#15106=CARTESIAN_POINT('Origin',(0.,15.,1.4));
#15107=CARTESIAN_POINT('Origin',(0.,15.,1.));
#15108=CARTESIAN_POINT('',(0.,0.,0.));
#15109=CARTESIAN_POINT('Origin',(0.,15.2,3.5));
#15110=CARTESIAN_POINT('',(-0.165,15.2,3.5));
#15111=CARTESIAN_POINT('Origin',(0.,15.2,3.5));
#15112=CARTESIAN_POINT('',(-0.165,16.3,3.5));
#15113=CARTESIAN_POINT('',(-0.165,15.2,3.5));
#15114=CARTESIAN_POINT('Origin',(0.,16.3,3.5));
#15115=CARTESIAN_POINT('Origin',(0.,15.2,3.5));
#15116=CARTESIAN_POINT('Origin',(0.,13.7,3.5));
#15117=CARTESIAN_POINT('',(-0.8,13.7,3.5));
#15118=CARTESIAN_POINT('Origin',(0.,13.7,3.5));
#15119=CARTESIAN_POINT('',(-0.5,13.7,3.5));
#15120=CARTESIAN_POINT('Origin',(0.,13.7,3.5));
#15121=CARTESIAN_POINT('Origin',(0.,13.3,3.5));
#15122=CARTESIAN_POINT('',(-0.8,13.3,3.5));
#15123=CARTESIAN_POINT('',(-0.8,13.3,3.5));
#15124=CARTESIAN_POINT('Origin',(0.,13.3,3.5));
#15125=CARTESIAN_POINT('Origin',(0.,13.3,3.5));
#15126=CARTESIAN_POINT('Origin',(0.,13.7,3.5));
#15127=CARTESIAN_POINT('',(-0.5,16.3,3.5));
#15128=CARTESIAN_POINT('Origin',(0.,16.3,3.5));
#15129=CARTESIAN_POINT('',(-0.5,13.7,3.5));
#15130=CARTESIAN_POINT('Origin',(0.,16.3,3.5));
#15131=CARTESIAN_POINT('',(0.,0.,0.));
#15132=CARTESIAN_POINT('Origin',(0.,14.1,3.5));
#15133=CARTESIAN_POINT('',(-0.505,14.55,3.5));
#15134=CARTESIAN_POINT('Origin',(0.,14.55,3.5));
#15135=CARTESIAN_POINT('',(-0.505,14.1,3.5));
#15136=CARTESIAN_POINT('',(-0.505,14.1,3.5));
#15137=CARTESIAN_POINT('Origin',(0.,14.1,3.5));
#15138=CARTESIAN_POINT('Origin',(0.,14.1,3.5));
#15139=CARTESIAN_POINT('',(-0.7,14.55,3.5));
#15140=CARTESIAN_POINT('Origin',(0.,14.55,3.5));
#15141=CARTESIAN_POINT('',(-0.7,14.1,3.5));
#15142=CARTESIAN_POINT('',(-0.7,14.1,3.5));
#15143=CARTESIAN_POINT('Origin',(0.,14.1,3.5));
#15144=CARTESIAN_POINT('Origin',(0.,14.55,3.5));
#15145=CARTESIAN_POINT('Origin',(0.,14.1,3.5));
#15146=CARTESIAN_POINT('',(0.,0.,0.));
#15147=CARTESIAN_POINT('Origin',(0.,15.45,3.5));
#15148=CARTESIAN_POINT('',(-0.505,15.9,3.5));
#15149=CARTESIAN_POINT('Origin',(0.,15.9,3.5));
#15150=CARTESIAN_POINT('',(-0.505,15.45,3.5));
#15151=CARTESIAN_POINT('',(-0.505,15.45,3.5));
#15152=CARTESIAN_POINT('Origin',(0.,15.45,3.5));
#15153=CARTESIAN_POINT('Origin',(0.,15.45,3.5));
#15154=CARTESIAN_POINT('',(-0.7,15.9,3.5));
#15155=CARTESIAN_POINT('Origin',(0.,15.9,3.5));
#15156=CARTESIAN_POINT('',(-0.7,15.45,3.5));
#15157=CARTESIAN_POINT('',(-0.7,15.45,3.5));
#15158=CARTESIAN_POINT('Origin',(0.,15.45,3.5));
#15159=CARTESIAN_POINT('Origin',(0.,15.9,3.5));
#15160=CARTESIAN_POINT('Origin',(0.,15.45,3.5));
#15161=CARTESIAN_POINT('',(0.,0.,0.));
#15162=CARTESIAN_POINT('Origin',(0.,16.3,3.5));
#15163=CARTESIAN_POINT('',(-0.225,16.5,3.5));
#15164=CARTESIAN_POINT('Origin',(0.,16.5,3.5));
#15165=CARTESIAN_POINT('',(-0.225,16.3,3.5));
#15166=CARTESIAN_POINT('',(-0.225,16.3,3.5));
#15167=CARTESIAN_POINT('Origin',(0.,16.3,3.5));
#15168=CARTESIAN_POINT('Origin',(0.,16.3,3.5));
#15169=CARTESIAN_POINT('',(-0.8,16.5,3.5));
#15170=CARTESIAN_POINT('Origin',(0.,16.5,3.5));
#15171=CARTESIAN_POINT('',(-0.8,16.3,3.5));
#15172=CARTESIAN_POINT('',(-0.8,16.3,3.5));
#15173=CARTESIAN_POINT('Origin',(0.,16.3,3.5));
#15174=CARTESIAN_POINT('Origin',(0.,16.5,3.5));
#15175=CARTESIAN_POINT('Origin',(0.,16.3,3.5));
#15176=CARTESIAN_POINT('',(0.,0.,0.));
#15177=CARTESIAN_POINT('Origin',(0.115470053837925,-0.5,-0.2));
#15178=CARTESIAN_POINT('',(0.23094010767585,-0.5,0.));
#15179=CARTESIAN_POINT('',(0.115470053837925,-0.5,-0.2));
#15180=CARTESIAN_POINT('',(0.23094010767585,-0.5,0.));
#15181=CARTESIAN_POINT('',(0.115470053837925,-0.8,-0.2));
#15182=CARTESIAN_POINT('',(0.115470053837925,-0.5,-0.2));
#15183=CARTESIAN_POINT('',(0.23094010767585,-0.8,0.));
#15184=CARTESIAN_POINT('',(0.23094010767585,-0.8,0.));
#15185=CARTESIAN_POINT('',(0.23094010767585,-0.5,0.));
#15186=CARTESIAN_POINT('Origin',(-0.115470053837925,-0.5,-0.2));
#15187=CARTESIAN_POINT('',(-0.115470053837925,-0.5,-0.2));
#15188=CARTESIAN_POINT('',(0.115470053837925,-0.5,-0.2));
#15189=CARTESIAN_POINT('',(-0.115470053837925,-0.8,-0.2));
#15190=CARTESIAN_POINT('',(-0.115470053837925,-0.5,-0.2));
#15191=CARTESIAN_POINT('',(0.115470053837925,-0.8,-0.2));
#15192=CARTESIAN_POINT('Origin',(-0.23094010767585,-0.5,-2.77555756156289E-17));
#15193=CARTESIAN_POINT('',(-0.23094010767585,-0.5,-2.82820063659975E-17));
#15194=CARTESIAN_POINT('',(-0.115470053837925,-0.5,-0.2));
#15195=CARTESIAN_POINT('',(-0.23094010767585,-0.8,-2.77555756156289E-17));
#15196=CARTESIAN_POINT('',(-0.23094010767585,-0.5,-2.82820063659975E-17));
#15197=CARTESIAN_POINT('',(-0.115470053837925,-0.8,-0.2));
#15198=CARTESIAN_POINT('Origin',(-0.115470053837925,-0.5,0.2));
#15199=CARTESIAN_POINT('',(-0.115470053837925,-0.5,0.2));
#15200=CARTESIAN_POINT('',(-0.23094010767585,-0.5,-2.82820063659975E-17));
#15201=CARTESIAN_POINT('',(-0.115470053837925,-0.8,0.2));
#15202=CARTESIAN_POINT('',(-0.115470053837925,-0.5,0.2));
#15203=CARTESIAN_POINT('',(-0.23094010767585,-0.8,-2.82820063659975E-17));
#15204=CARTESIAN_POINT('Origin',(0.115470053837925,-0.5,0.2));
#15205=CARTESIAN_POINT('',(0.115470053837925,-0.5,0.2));
#15206=CARTESIAN_POINT('',(-0.115470053837925,-0.5,0.2));
#15207=CARTESIAN_POINT('',(0.115470053837925,-0.8,0.2));
#15208=CARTESIAN_POINT('',(0.115470053837925,-0.5,0.2));
#15209=CARTESIAN_POINT('',(-0.115470053837925,-0.8,0.2));
#15210=CARTESIAN_POINT('Origin',(0.23094010767585,-0.5,0.));
#15211=CARTESIAN_POINT('',(0.115470053837925,-0.5,0.2));
#15212=CARTESIAN_POINT('',(0.115470053837925,-0.8,0.2));
#15213=CARTESIAN_POINT('Origin',(0.,-0.5,0.));
#15214=CARTESIAN_POINT('Origin',(0.,-0.8,0.));
#15215=CARTESIAN_POINT('Origin',(0.,-1.4,0.));
#15216=CARTESIAN_POINT('',(-0.24505,-1.4,3.00099698131059E-17));
#15217=CARTESIAN_POINT('Origin',(0.,-1.4,0.));
#15218=CARTESIAN_POINT('Origin',(0.375,0.5,0.));
#15219=CARTESIAN_POINT('',(-0.375,0.5,-4.59242549680257E-17));
#15220=CARTESIAN_POINT('Origin',(0.,0.5,0.));
#15221=CARTESIAN_POINT('Origin',(0.,0.475,0.));
#15222=CARTESIAN_POINT('',(-0.425,0.45,-5.20474889637625E-17));
#15223=CARTESIAN_POINT('Origin',(0.,0.45,0.));
#15224=CARTESIAN_POINT('',(-0.4,0.475,-4.89858719658941E-17));
#15225=CARTESIAN_POINT('Origin',(0.,0.24,0.));
#15226=CARTESIAN_POINT('',(-0.425,0.0299999999999998,-5.20474889637625E-17));
#15227=CARTESIAN_POINT('Origin',(0.,0.0299999999999998,0.));
#15228=CARTESIAN_POINT('',(-0.425,0.24,-5.20474889637625E-17));
#15229=CARTESIAN_POINT('Origin',(0.,0.0150000000000001,0.));
#15230=CARTESIAN_POINT('',(-0.395,4.85722573273506E-17,-4.83735485663204E-17));
#15231=CARTESIAN_POINT('Origin',(0.,0.,0.));
#15232=CARTESIAN_POINT('',(-0.41,0.0150000000000001,-5.02105187650415E-17));
#15233=CARTESIAN_POINT('Origin',(0.27,0.,0.));
#15234=CARTESIAN_POINT('',(-0.27,0.,-3.30654635769785E-17));
#15235=CARTESIAN_POINT('Origin',(0.,0.,0.));
#15236=CARTESIAN_POINT('Origin',(0.,-0.02,0.));
#15237=CARTESIAN_POINT('',(-0.24505,-0.0498999999999999,3.00099698131059E-17));
#15238=CARTESIAN_POINT('Origin',(0.,-0.0498999999999999,0.));
#15239=CARTESIAN_POINT('',(-0.26,-0.02,-3.18408167778312E-17));
#15240=CARTESIAN_POINT('Origin',(0.,-0.995,0.));
#15241=CARTESIAN_POINT('',(-0.24505,-0.995,-3.00099698131059E-17));
#15242=CARTESIAN_POINT('',(0.,0.,0.));
#15243=CARTESIAN_POINT('Origin',(0.0866025403784439,-0.4,-0.15));
#15244=CARTESIAN_POINT('',(0.173205080756888,-0.4,0.));
#15245=CARTESIAN_POINT('',(0.0866025403784439,-0.4,-0.15));
#15246=CARTESIAN_POINT('',(0.173205080756888,-0.4,0.));
#15247=CARTESIAN_POINT('',(0.0866025403784439,-0.64,-0.15));
#15248=CARTESIAN_POINT('',(0.0866025403784439,-0.4,-0.15));
#15249=CARTESIAN_POINT('',(0.173205080756888,-0.64,0.));
#15250=CARTESIAN_POINT('',(0.173205080756888,-0.64,0.));
#15251=CARTESIAN_POINT('',(0.173205080756888,-0.4,0.));
#15252=CARTESIAN_POINT('Origin',(-0.0866025403784438,-0.4,-0.15));
#15253=CARTESIAN_POINT('',(-0.0866025403784438,-0.4,-0.15));
#15254=CARTESIAN_POINT('',(0.0866025403784439,-0.4,-0.15));
#15255=CARTESIAN_POINT('',(-0.0866025403784438,-0.64,-0.15));
#15256=CARTESIAN_POINT('',(-0.0866025403784438,-0.4,-0.15));
#15257=CARTESIAN_POINT('',(0.0866025403784439,-0.64,-0.15));
#15258=CARTESIAN_POINT('Origin',(-0.173205080756888,-0.4,-2.77555756156289E-17));
#15259=CARTESIAN_POINT('',(-0.173205080756888,-0.4,-2.12115047744981E-17));
#15260=CARTESIAN_POINT('',(-0.0866025403784438,-0.4,-0.15));
#15261=CARTESIAN_POINT('',(-0.173205080756888,-0.64,-2.77555756156289E-17));
#15262=CARTESIAN_POINT('',(-0.173205080756888,-0.4,-2.12115047744981E-17));
#15263=CARTESIAN_POINT('',(-0.0866025403784438,-0.64,-0.15));
#15264=CARTESIAN_POINT('Origin',(-0.0866025403784439,-0.4,0.15));
#15265=CARTESIAN_POINT('',(-0.0866025403784439,-0.4,0.15));
#15266=CARTESIAN_POINT('',(-0.173205080756888,-0.4,-2.12115047744981E-17));
#15267=CARTESIAN_POINT('',(-0.0866025403784439,-0.64,0.15));
#15268=CARTESIAN_POINT('',(-0.0866025403784439,-0.4,0.15));
#15269=CARTESIAN_POINT('',(-0.173205080756888,-0.64,-2.12115047744981E-17));
#15270=CARTESIAN_POINT('Origin',(0.0866025403784439,-0.4,0.15));
#15271=CARTESIAN_POINT('',(0.0866025403784439,-0.4,0.15));
#15272=CARTESIAN_POINT('',(-0.0866025403784439,-0.4,0.15));
#15273=CARTESIAN_POINT('',(0.0866025403784439,-0.64,0.15));
#15274=CARTESIAN_POINT('',(0.0866025403784439,-0.4,0.15));
#15275=CARTESIAN_POINT('',(-0.0866025403784439,-0.64,0.15));
#15276=CARTESIAN_POINT('Origin',(0.173205080756888,-0.4,0.));
#15277=CARTESIAN_POINT('',(0.0866025403784439,-0.4,0.15));
#15278=CARTESIAN_POINT('',(0.0866025403784439,-0.64,0.15));
#15279=CARTESIAN_POINT('Origin',(0.,-0.4,-2.77555756156289E-17));
#15280=CARTESIAN_POINT('Origin',(0.,-0.64,-2.77555756156289E-17));
#15281=CARTESIAN_POINT('Origin',(0.,-1.,0.));
#15282=CARTESIAN_POINT('',(-0.1954,-1.,2.39295984553393E-17));
#15283=CARTESIAN_POINT('Origin',(0.,-1.,0.));
#15284=CARTESIAN_POINT('Origin',(0.3,0.4,0.));
#15285=CARTESIAN_POINT('',(-0.3,0.4,-3.67394039744206E-17));
#15286=CARTESIAN_POINT('Origin',(0.,0.4,0.));
#15287=CARTESIAN_POINT('Origin',(0.,0.375,0.));
#15288=CARTESIAN_POINT('',(-0.35,0.35,-4.28626379701573E-17));
#15289=CARTESIAN_POINT('Origin',(0.,0.35,0.));
#15290=CARTESIAN_POINT('',(-0.325,0.375,-3.9801020972289E-17));
#15291=CARTESIAN_POINT('Origin',(0.,0.19,0.));
#15292=CARTESIAN_POINT('',(-0.35,0.03,-4.28626379701574E-17));
#15293=CARTESIAN_POINT('Origin',(0.,0.03,0.));
#15294=CARTESIAN_POINT('',(-0.35,0.19,-4.28626379701574E-17));
#15295=CARTESIAN_POINT('Origin',(0.,0.0149999999999999,0.));
#15296=CARTESIAN_POINT('',(-0.32,-3.29597460435593E-17,-3.91886975727153E-17));
#15297=CARTESIAN_POINT('Origin',(0.,0.,0.));
#15298=CARTESIAN_POINT('',(-0.335,0.0149999999999999,-4.10256677714363E-17));
#15299=CARTESIAN_POINT('Origin',(0.22,0.,0.));
#15300=CARTESIAN_POINT('',(-0.22,-6.93889390390723E-18,-2.69422295812418E-17));
#15301=CARTESIAN_POINT('Origin',(0.,0.,0.));
#15302=CARTESIAN_POINT('Origin',(0.,-0.02,0.));
#15303=CARTESIAN_POINT('',(-0.1954,-0.0492,2.39295984553393E-17));
#15304=CARTESIAN_POINT('Origin',(0.,-0.0492,0.));
#15305=CARTESIAN_POINT('',(-0.21,-0.02,-2.57175827820944E-17));
#15306=CARTESIAN_POINT('Origin',(0.,-0.8,0.));
#15307=CARTESIAN_POINT('',(-0.1954,-0.8,-2.39295984553393E-17));
#15308=CARTESIAN_POINT('',(0.,0.,0.));
#15309=CARTESIAN_POINT('',(0.,0.,0.));
#15310=CARTESIAN_POINT('',(0.,0.,0.));
#15311=CARTESIAN_POINT('',(0.,0.,0.));
#15312=CARTESIAN_POINT('',(0.,0.,0.));
#15313=CARTESIAN_POINT('',(-1.8,13.,1.4));
#15314=CARTESIAN_POINT('',(-1.8,17.,1.4));
#15315=CARTESIAN_POINT('',(1.8,13.,1.4));
#15316=CARTESIAN_POINT('',(1.8,17.,1.4));
#15317=CARTESIAN_POINT('',(0.,16.5,3.5));
#15318=CARTESIAN_POINT('',(0.,0.,0.));
#15319=CARTESIAN_POINT('',(0.,0.,0.));
#15320=CARTESIAN_POINT('',(0.,0.,0.));
#15321=CARTESIAN_POINT('',(0.,0.,0.));
#15322=CARTESIAN_POINT('',(0.,0.,0.));
#15323=CARTESIAN_POINT('',(-1.8,13.,1.4));
#15324=CARTESIAN_POINT('',(-1.8,17.,1.4));
#15325=CARTESIAN_POINT('',(1.8,13.,1.4));
#15326=CARTESIAN_POINT('',(1.8,17.,1.4));
#15327=CARTESIAN_POINT('',(0.,16.5,3.5));
#15328=CARTESIAN_POINT('',(0.,0.,0.));
#15329=CARTESIAN_POINT('',(0.,0.,0.));
#15330=CARTESIAN_POINT('',(0.,0.,0.));
#15331=CARTESIAN_POINT('',(0.,0.,0.));
#15332=CARTESIAN_POINT('',(0.,0.,0.));
#15333=CARTESIAN_POINT('',(-1.8,13.,1.4));
#15334=CARTESIAN_POINT('',(-1.8,17.,1.4));
#15335=CARTESIAN_POINT('',(1.8,13.,1.4));
#15336=CARTESIAN_POINT('',(1.8,17.,1.4));
#15337=CARTESIAN_POINT('',(0.,16.5,3.5));
#15338=CARTESIAN_POINT('',(0.,0.,0.));
#15339=CARTESIAN_POINT('',(0.,0.,0.));
#15340=CARTESIAN_POINT('',(0.,0.,0.));
#15341=CARTESIAN_POINT('',(0.,0.,0.));
#15342=CARTESIAN_POINT('',(0.,0.,0.));
#15343=CARTESIAN_POINT('',(-1.8,13.,1.4));
#15344=CARTESIAN_POINT('',(-1.8,17.,1.4));
#15345=CARTESIAN_POINT('',(1.8,13.,1.4));
#15346=CARTESIAN_POINT('',(1.8,17.,1.4));
#15347=CARTESIAN_POINT('',(0.,16.5,3.5));
#15348=CARTESIAN_POINT('',(0.,0.,0.));
#15349=CARTESIAN_POINT('',(0.,0.,0.));
#15350=CARTESIAN_POINT('Origin',(0.,14.35,3.5));
#15351=CARTESIAN_POINT('',(-1.5,15.65,3.5));
#15352=CARTESIAN_POINT('Origin',(0.,15.65,3.5));
#15353=CARTESIAN_POINT('',(-1.5,14.35,3.5));
#15354=CARTESIAN_POINT('',(-1.5,14.35,3.5));
#15355=CARTESIAN_POINT('Origin',(0.,14.35,3.5));
#15356=CARTESIAN_POINT('Origin',(0.,14.35,3.5));
#15357=CARTESIAN_POINT('',(-2.,15.65,3.5));
#15358=CARTESIAN_POINT('Origin',(0.,15.65,3.5));
#15359=CARTESIAN_POINT('',(-2.,14.35,3.5));
#15360=CARTESIAN_POINT('',(-2.,14.35,3.5));
#15361=CARTESIAN_POINT('Origin',(0.,14.35,3.5));
#15362=CARTESIAN_POINT('Origin',(0.,15.65,3.5));
#15363=CARTESIAN_POINT('Origin',(0.,14.35,3.5));
#15364=CARTESIAN_POINT('',(0.,0.,0.));
#15365=CARTESIAN_POINT('Origin',(0.,14.35,3.5));
#15366=CARTESIAN_POINT('',(-1.1,14.55,3.5));
#15367=CARTESIAN_POINT('Origin',(0.,14.55,3.5));
#15368=CARTESIAN_POINT('',(-1.1,14.35,3.5));
#15369=CARTESIAN_POINT('',(-1.1,14.35,3.5));
#15370=CARTESIAN_POINT('Origin',(0.,14.35,3.5));
#15371=CARTESIAN_POINT('Origin',(0.,14.35,3.5));
#15372=CARTESIAN_POINT('',(-1.5,14.55,3.5));
#15373=CARTESIAN_POINT('Origin',(0.,14.55,3.5));
#15374=CARTESIAN_POINT('',(-1.5,14.35,3.5));
#15375=CARTESIAN_POINT('',(-1.5,14.35,3.5));
#15376=CARTESIAN_POINT('Origin',(0.,14.35,3.5));
#15377=CARTESIAN_POINT('Origin',(0.,14.55,3.5));
#15378=CARTESIAN_POINT('Origin',(0.,14.35,3.5));
#15379=CARTESIAN_POINT('',(0.,0.,0.));
#15380=CARTESIAN_POINT('Origin',(0.,15.45,3.5));
#15381=CARTESIAN_POINT('',(-1.1,15.65,3.5));
#15382=CARTESIAN_POINT('Origin',(0.,15.65,3.5));
#15383=CARTESIAN_POINT('',(-1.1,15.45,3.5));
#15384=CARTESIAN_POINT('',(-1.1,15.45,3.5));
#15385=CARTESIAN_POINT('Origin',(0.,15.45,3.5));
#15386=CARTESIAN_POINT('Origin',(0.,15.45,3.5));
#15387=CARTESIAN_POINT('',(-1.5,15.65,3.5));
#15388=CARTESIAN_POINT('Origin',(0.,15.65,3.5));
#15389=CARTESIAN_POINT('',(-1.5,15.45,3.5));
#15390=CARTESIAN_POINT('',(-1.5,15.45,3.5));
#15391=CARTESIAN_POINT('Origin',(0.,15.45,3.5));
#15392=CARTESIAN_POINT('Origin',(0.,15.65,3.5));
#15393=CARTESIAN_POINT('Origin',(0.,15.45,3.5));
#15394=CARTESIAN_POINT('',(0.,0.,0.));
#15395=CARTESIAN_POINT('',(0.,0.,0.));
#15396=CARTESIAN_POINT('Origin',(0.,14.35,3.5));
#15397=CARTESIAN_POINT('',(-1.5,15.65,3.5));
#15398=CARTESIAN_POINT('Origin',(0.,15.65,3.5));
#15399=CARTESIAN_POINT('',(-1.5,14.35,3.5));
#15400=CARTESIAN_POINT('',(-1.5,14.35,3.5));
#15401=CARTESIAN_POINT('Origin',(0.,14.35,3.5));
#15402=CARTESIAN_POINT('Origin',(0.,14.35,3.5));
#15403=CARTESIAN_POINT('',(-2.,15.65,3.5));
#15404=CARTESIAN_POINT('Origin',(0.,15.65,3.5));
#15405=CARTESIAN_POINT('',(-2.,14.35,3.5));
#15406=CARTESIAN_POINT('',(-2.,14.35,3.5));
#15407=CARTESIAN_POINT('Origin',(0.,14.35,3.5));
#15408=CARTESIAN_POINT('Origin',(0.,15.65,3.5));
#15409=CARTESIAN_POINT('Origin',(0.,14.35,3.5));
#15410=CARTESIAN_POINT('',(0.,0.,0.));
#15411=CARTESIAN_POINT('Origin',(0.,14.35,3.5));
#15412=CARTESIAN_POINT('',(-1.1,14.55,3.5));
#15413=CARTESIAN_POINT('Origin',(0.,14.55,3.5));
#15414=CARTESIAN_POINT('',(-1.1,14.35,3.5));
#15415=CARTESIAN_POINT('',(-1.1,14.35,3.5));
#15416=CARTESIAN_POINT('Origin',(0.,14.35,3.5));
#15417=CARTESIAN_POINT('Origin',(0.,14.35,3.5));
#15418=CARTESIAN_POINT('',(-1.5,14.55,3.5));
#15419=CARTESIAN_POINT('Origin',(0.,14.55,3.5));
#15420=CARTESIAN_POINT('',(-1.5,14.35,3.5));
#15421=CARTESIAN_POINT('',(-1.5,14.35,3.5));
#15422=CARTESIAN_POINT('Origin',(0.,14.35,3.5));
#15423=CARTESIAN_POINT('Origin',(0.,14.55,3.5));
#15424=CARTESIAN_POINT('Origin',(0.,14.35,3.5));
#15425=CARTESIAN_POINT('',(0.,0.,0.));
#15426=CARTESIAN_POINT('Origin',(0.,15.45,3.5));
#15427=CARTESIAN_POINT('',(-1.1,15.65,3.5));
#15428=CARTESIAN_POINT('Origin',(0.,15.65,3.5));
#15429=CARTESIAN_POINT('',(-1.1,15.45,3.5));
#15430=CARTESIAN_POINT('',(-1.1,15.45,3.5));
#15431=CARTESIAN_POINT('Origin',(0.,15.45,3.5));
#15432=CARTESIAN_POINT('Origin',(0.,15.45,3.5));
#15433=CARTESIAN_POINT('',(-1.5,15.65,3.5));
#15434=CARTESIAN_POINT('Origin',(0.,15.65,3.5));
#15435=CARTESIAN_POINT('',(-1.5,15.45,3.5));
#15436=CARTESIAN_POINT('',(-1.5,15.45,3.5));
#15437=CARTESIAN_POINT('Origin',(0.,15.45,3.5));
#15438=CARTESIAN_POINT('Origin',(0.,15.65,3.5));
#15439=CARTESIAN_POINT('Origin',(0.,15.45,3.5));
#15440=CARTESIAN_POINT('',(0.,0.,0.));
#15441=CARTESIAN_POINT('',(0.,0.,0.));
#15442=CARTESIAN_POINT('Origin',(0.,14.35,3.5));
#15443=CARTESIAN_POINT('',(-1.5,15.65,3.5));
#15444=CARTESIAN_POINT('Origin',(0.,15.65,3.5));
#15445=CARTESIAN_POINT('',(-1.5,14.35,3.5));
#15446=CARTESIAN_POINT('',(-1.5,14.35,3.5));
#15447=CARTESIAN_POINT('Origin',(0.,14.35,3.5));
#15448=CARTESIAN_POINT('Origin',(0.,14.35,3.5));
#15449=CARTESIAN_POINT('',(-2.,15.65,3.5));
#15450=CARTESIAN_POINT('Origin',(0.,15.65,3.5));
#15451=CARTESIAN_POINT('',(-2.,14.35,3.5));
#15452=CARTESIAN_POINT('',(-2.,14.35,3.5));
#15453=CARTESIAN_POINT('Origin',(0.,14.35,3.5));
#15454=CARTESIAN_POINT('Origin',(0.,15.65,3.5));
#15455=CARTESIAN_POINT('Origin',(0.,14.35,3.5));
#15456=CARTESIAN_POINT('',(0.,0.,0.));
#15457=CARTESIAN_POINT('Origin',(0.,14.35,3.5));
#15458=CARTESIAN_POINT('',(-1.1,14.55,3.5));
#15459=CARTESIAN_POINT('Origin',(0.,14.55,3.5));
#15460=CARTESIAN_POINT('',(-1.1,14.35,3.5));
#15461=CARTESIAN_POINT('',(-1.1,14.35,3.5));
#15462=CARTESIAN_POINT('Origin',(0.,14.35,3.5));
#15463=CARTESIAN_POINT('Origin',(0.,14.35,3.5));
#15464=CARTESIAN_POINT('',(-1.5,14.55,3.5));
#15465=CARTESIAN_POINT('Origin',(0.,14.55,3.5));
#15466=CARTESIAN_POINT('',(-1.5,14.35,3.5));
#15467=CARTESIAN_POINT('',(-1.5,14.35,3.5));
#15468=CARTESIAN_POINT('Origin',(0.,14.35,3.5));
#15469=CARTESIAN_POINT('Origin',(0.,14.55,3.5));
#15470=CARTESIAN_POINT('Origin',(0.,14.35,3.5));
#15471=CARTESIAN_POINT('',(0.,0.,0.));
#15472=CARTESIAN_POINT('Origin',(0.,15.45,3.5));
#15473=CARTESIAN_POINT('',(-1.1,15.65,3.5));
#15474=CARTESIAN_POINT('Origin',(0.,15.65,3.5));
#15475=CARTESIAN_POINT('',(-1.1,15.45,3.5));
#15476=CARTESIAN_POINT('',(-1.1,15.45,3.5));
#15477=CARTESIAN_POINT('Origin',(0.,15.45,3.5));
#15478=CARTESIAN_POINT('Origin',(0.,15.45,3.5));
#15479=CARTESIAN_POINT('',(-1.5,15.65,3.5));
#15480=CARTESIAN_POINT('Origin',(0.,15.65,3.5));
#15481=CARTESIAN_POINT('',(-1.5,15.45,3.5));
#15482=CARTESIAN_POINT('',(-1.5,15.45,3.5));
#15483=CARTESIAN_POINT('Origin',(0.,15.45,3.5));
#15484=CARTESIAN_POINT('Origin',(0.,15.65,3.5));
#15485=CARTESIAN_POINT('Origin',(0.,15.45,3.5));
#15486=CARTESIAN_POINT('',(0.,0.,0.));
#15487=CARTESIAN_POINT('',(0.,0.,0.));
#15488=CARTESIAN_POINT('Origin',(0.,14.35,3.5));
#15489=CARTESIAN_POINT('',(-1.5,15.65,3.5));
#15490=CARTESIAN_POINT('Origin',(0.,15.65,3.5));
#15491=CARTESIAN_POINT('',(-1.5,14.35,3.5));
#15492=CARTESIAN_POINT('',(-1.5,14.35,3.5));
#15493=CARTESIAN_POINT('Origin',(0.,14.35,3.5));
#15494=CARTESIAN_POINT('Origin',(0.,14.35,3.5));
#15495=CARTESIAN_POINT('',(-2.,15.65,3.5));
#15496=CARTESIAN_POINT('Origin',(0.,15.65,3.5));
#15497=CARTESIAN_POINT('',(-2.,14.35,3.5));
#15498=CARTESIAN_POINT('',(-2.,14.35,3.5));
#15499=CARTESIAN_POINT('Origin',(0.,14.35,3.5));
#15500=CARTESIAN_POINT('Origin',(0.,15.65,3.5));
#15501=CARTESIAN_POINT('Origin',(0.,14.35,3.5));
#15502=CARTESIAN_POINT('',(0.,0.,0.));
#15503=CARTESIAN_POINT('Origin',(0.,14.35,3.5));
#15504=CARTESIAN_POINT('',(-1.1,14.55,3.5));
#15505=CARTESIAN_POINT('Origin',(0.,14.55,3.5));
#15506=CARTESIAN_POINT('',(-1.1,14.35,3.5));
#15507=CARTESIAN_POINT('',(-1.1,14.35,3.5));
#15508=CARTESIAN_POINT('Origin',(0.,14.35,3.5));
#15509=CARTESIAN_POINT('Origin',(0.,14.35,3.5));
#15510=CARTESIAN_POINT('',(-1.5,14.55,3.5));
#15511=CARTESIAN_POINT('Origin',(0.,14.55,3.5));
#15512=CARTESIAN_POINT('',(-1.5,14.35,3.5));
#15513=CARTESIAN_POINT('',(-1.5,14.35,3.5));
#15514=CARTESIAN_POINT('Origin',(0.,14.35,3.5));
#15515=CARTESIAN_POINT('Origin',(0.,14.55,3.5));
#15516=CARTESIAN_POINT('Origin',(0.,14.35,3.5));
#15517=CARTESIAN_POINT('',(0.,0.,0.));
#15518=CARTESIAN_POINT('Origin',(0.,15.45,3.5));
#15519=CARTESIAN_POINT('',(-1.1,15.65,3.5));
#15520=CARTESIAN_POINT('Origin',(0.,15.65,3.5));
#15521=CARTESIAN_POINT('',(-1.1,15.45,3.5));
#15522=CARTESIAN_POINT('',(-1.1,15.45,3.5));
#15523=CARTESIAN_POINT('Origin',(0.,15.45,3.5));
#15524=CARTESIAN_POINT('Origin',(0.,15.45,3.5));
#15525=CARTESIAN_POINT('',(-1.5,15.65,3.5));
#15526=CARTESIAN_POINT('Origin',(0.,15.65,3.5));
#15527=CARTESIAN_POINT('',(-1.5,15.45,3.5));
#15528=CARTESIAN_POINT('',(-1.5,15.45,3.5));
#15529=CARTESIAN_POINT('Origin',(0.,15.45,3.5));
#15530=CARTESIAN_POINT('Origin',(0.,15.65,3.5));
#15531=CARTESIAN_POINT('Origin',(0.,15.45,3.5));
#15532=CARTESIAN_POINT('',(0.,0.,0.));
#15533=CARTESIAN_POINT('',(0.,0.,0.));
#15534=CARTESIAN_POINT('Origin',(0.,0.,0.));
#15535=CARTESIAN_POINT('',(-0.976185,-0.246528389340863,-1.19548183562566E-16));
#15536=CARTESIAN_POINT('',(-1.19548183562566E-16,-0.246528389340863,0.976185));
#15537=CARTESIAN_POINT('Origin',(0.,-0.246528389340863,0.));
#15538=CARTESIAN_POINT('Origin',(0.,-0.246528389340863,0.));
#15539=CARTESIAN_POINT('',(-1.19548183562566E-16,0.246528389340863,0.976185));
#15540=CARTESIAN_POINT('Origin',(-1.22464679914735E-16,0.,1.));
#15541=CARTESIAN_POINT('',(-0.976185,0.246528389340863,1.19548183562566E-16));
#15542=CARTESIAN_POINT('Origin',(0.,0.246528389340863,0.));
#15543=CARTESIAN_POINT('Origin',(0.,0.246528389340863,0.));
#15544=CARTESIAN_POINT('Origin',(0.,0.,0.));
#15545=CARTESIAN_POINT('',(-0.976185,0.45,-1.19548183562566E-16));
#15546=CARTESIAN_POINT('',(-0.976185,0.,-1.19548183562566E-16));
#15547=CARTESIAN_POINT('Origin',(0.,0.45,0.));
#15548=CARTESIAN_POINT('Origin',(0.,0.,0.));
#15549=CARTESIAN_POINT('',(-0.5,-0.39,-6.12323399573677E-17));
#15550=CARTESIAN_POINT('Origin',(0.,-0.39,0.));
#15551=CARTESIAN_POINT('',(-0.5,0.39,-6.12323399573677E-17));
#15552=CARTESIAN_POINT('',(-0.5,0.,-6.12323399573677E-17));
#15553=CARTESIAN_POINT('Origin',(0.,0.39,0.));
#15554=CARTESIAN_POINT('Origin',(0.,0.42,0.));
#15555=CARTESIAN_POINT('',(-0.56,0.45,-6.85802207522518E-17));
#15556=CARTESIAN_POINT('',(-0.53,0.42,-6.49062803548097E-17));
#15557=CARTESIAN_POINT('Origin',(0.,0.45,0.));
#15558=CARTESIAN_POINT('Origin',(0.976185,0.45,0.));
#15559=CARTESIAN_POINT('Origin',(0.,0.,0.));
#15560=CARTESIAN_POINT('',(-0.976185,-0.45,-1.19548183562566E-16));
#15561=CARTESIAN_POINT('Origin',(0.,-0.45,0.));
#15562=CARTESIAN_POINT('',(-0.976185,0.,-1.19548183562566E-16));
#15563=CARTESIAN_POINT('Origin',(0.56,-0.45,0.));
#15564=CARTESIAN_POINT('',(-0.56,-0.45,-6.85802207522518E-17));
#15565=CARTESIAN_POINT('Origin',(0.,-0.45,0.));
#15566=CARTESIAN_POINT('Origin',(0.,-0.42,0.));
#15567=CARTESIAN_POINT('',(-0.53,-0.42,-6.49062803548097E-17));
#15568=CARTESIAN_POINT('',(0.,0.,0.));
#15569=CARTESIAN_POINT('Origin',(0.,0.,0.));
#15570=CARTESIAN_POINT('',(-1.023815,0.246528389340863,-1.25381176266905E-16));
#15571=CARTESIAN_POINT('',(-1.25381176266905E-16,0.246528389340863,1.023815));
#15572=CARTESIAN_POINT('Origin',(0.,0.246528389340863,0.));
#15573=CARTESIAN_POINT('Origin',(0.,0.246528389340863,0.));
#15574=CARTESIAN_POINT('',(-1.25381176266905E-16,-0.246528389340863,1.023815));
#15575=CARTESIAN_POINT('Origin',(-1.22464679914735E-16,0.,1.));
#15576=CARTESIAN_POINT('',(-1.023815,-0.246528389340863,1.25381176266905E-16));
#15577=CARTESIAN_POINT('Origin',(0.,-0.246528389340863,0.));
#15578=CARTESIAN_POINT('Origin',(0.,-0.246528389340863,0.));
#15579=CARTESIAN_POINT('Origin',(0.,0.,0.));
#15580=CARTESIAN_POINT('',(-1.023815,-0.45,-1.25381176266905E-16));
#15581=CARTESIAN_POINT('Origin',(0.,-0.45,0.));
#15582=CARTESIAN_POINT('',(-1.023815,0.,-1.25381176266905E-16));
#15583=CARTESIAN_POINT('Origin',(1.44,0.45,0.));
#15584=CARTESIAN_POINT('',(-1.44,0.45,-1.76349139077219E-16));
#15585=CARTESIAN_POINT('Origin',(0.,0.45,0.));
#15586=CARTESIAN_POINT('',(-1.023815,0.45,-1.25381176266905E-16));
#15587=CARTESIAN_POINT('Origin',(0.,0.45,0.));
#15588=CARTESIAN_POINT('Origin',(0.,0.42,0.));
#15589=CARTESIAN_POINT('',(-1.5,0.39,-1.83697019872103E-16));
#15590=CARTESIAN_POINT('Origin',(0.,0.39,0.));
#15591=CARTESIAN_POINT('',(-1.47,0.42,-1.80023079474661E-16));
#15592=CARTESIAN_POINT('Origin',(0.,0.,0.));
#15593=CARTESIAN_POINT('',(-1.5,-0.39,-1.83697019872103E-16));
#15594=CARTESIAN_POINT('Origin',(0.,-0.39,0.));
#15595=CARTESIAN_POINT('',(-1.5,0.,-1.83697019872103E-16));
#15596=CARTESIAN_POINT('Origin',(0.,-0.42,0.));
#15597=CARTESIAN_POINT('',(-1.44,-0.45,-1.76349139077219E-16));
#15598=CARTESIAN_POINT('Origin',(0.,-0.45,0.));
#15599=CARTESIAN_POINT('',(-1.47,-0.42,-1.80023079474661E-16));
#15600=CARTESIAN_POINT('Origin',(1.023815,-0.45,0.));
#15601=CARTESIAN_POINT('Origin',(0.,0.,0.));
#15602=CARTESIAN_POINT('',(-1.023815,0.,-1.25381176266905E-16));
#15603=CARTESIAN_POINT('',(0.,0.,0.));
#15604=CARTESIAN_POINT('Origin',(1.,0.,0.));
#15605=CARTESIAN_POINT('',(1.,-1.78583896120461E-33,0.23815));
#15606=CARTESIAN_POINT('',(1.,-1.78583896120461E-33,-0.23815));
#15607=CARTESIAN_POINT('Origin',(1.,0.,0.));
#15608=CARTESIAN_POINT('Origin',(0.707106781186548,0.,-0.707106781186547));
#15609=CARTESIAN_POINT('',(0.875504261126124,-1.78583896120461E-33,-0.538709301246971));
#15610=CARTESIAN_POINT('',(0.538709301246971,-1.78583896120461E-33,-0.875504261126124));
#15611=CARTESIAN_POINT('Origin',(0.707106781186548,0.,-0.707106781186547));
#15612=CARTESIAN_POINT('Origin',(6.12323399573677E-17,0.,-1.));
#15613=CARTESIAN_POINT('',(0.23815,-1.78583896120461E-33,-1.));
#15614=CARTESIAN_POINT('',(-0.23815,-1.78583896120461E-33,-1.));
#15615=CARTESIAN_POINT('Origin',(6.12323399573677E-17,0.,-1.));
#15616=CARTESIAN_POINT('Origin',(-0.707106781186547,0.,-0.707106781186548));
#15617=CARTESIAN_POINT('',(-0.538709301246971,-1.78583896120461E-33,-0.875504261126124));
#15618=CARTESIAN_POINT('',(-0.875504261126124,-1.78583896120461E-33,-0.538709301246971));
#15619=CARTESIAN_POINT('Origin',(-0.707106781186547,0.,-0.707106781186548));
#15620=CARTESIAN_POINT('Origin',(-1.,0.,-1.22464679914735E-16));
#15621=CARTESIAN_POINT('',(-1.,-1.78583896120461E-33,-0.23815));
#15622=CARTESIAN_POINT('',(-1.,-1.78583896120461E-33,0.23815));
#15623=CARTESIAN_POINT('Origin',(-1.,0.,-1.22464679914735E-16));
#15624=CARTESIAN_POINT('Origin',(-0.707106781186548,0.,0.707106781186547));
#15625=CARTESIAN_POINT('',(-0.875504261126124,-7.94881478324376E-33,0.538709301246971));
#15626=CARTESIAN_POINT('',(-0.538709301246971,4.37713686083455E-33,0.875504261126124));
#15627=CARTESIAN_POINT('Origin',(-0.707106781186548,0.,0.707106781186547));
#15628=CARTESIAN_POINT('Origin',(-1.83697019872103E-16,0.,1.));
#15629=CARTESIAN_POINT('',(-0.23815,-1.78583896120461E-33,1.));
#15630=CARTESIAN_POINT('',(0.23815,-1.78583896120461E-33,1.));
#15631=CARTESIAN_POINT('Origin',(-1.83697019872103E-16,0.,1.));
#15632=CARTESIAN_POINT('Origin',(0.707106781186547,0.,0.707106781186548));
#15633=CARTESIAN_POINT('',(0.538709301246971,-4.86732687222419E-33,0.875504261126124));
#15634=CARTESIAN_POINT('',(0.875504261126124,1.29564894981497E-33,0.538709301246971));
#15635=CARTESIAN_POINT('Origin',(0.707106781186547,0.,0.707106781186548));
#15636=CARTESIAN_POINT('',(0.,0.,0.));
#15637=CARTESIAN_POINT('Origin',(0.707106781186547,0.,0.707106781186548));
#15638=CARTESIAN_POINT('',(0.504455939115715,-0.04763,0.841298510752802));
#15639=CARTESIAN_POINT('',(0.841298510752802,-0.04763,0.504455939115715));
#15640=CARTESIAN_POINT('Ctrl Pts',(0.504455939115715,-0.04763,0.841298510752802));
#15641=CARTESIAN_POINT('Ctrl Pts',(0.508899795931835,-0.0740444353928835,
0.838633903678357));
#15642=CARTESIAN_POINT('Ctrl Pts',(0.517157748491652,-0.0999305678883309,
0.833661031856294));
#15643=CARTESIAN_POINT('Ctrl Pts',(0.537715343527944,-0.142345102874864,
0.820511285096538));
#15644=CARTESIAN_POINT('Ctrl Pts',(0.548874290046456,-0.159766064500479,
0.813159949759));
#15645=CARTESIAN_POINT('Ctrl Pts',(0.573915184558107,-0.190326085855194,
0.795684265985089));
#15646=CARTESIAN_POINT('Ctrl Pts',(0.587792702767295,-0.203463743702801,
0.78555112003688));
#15647=CARTESIAN_POINT('Ctrl Pts',(0.615966552324775,-0.224161999508995,
0.763642258217233));
#15648=CARTESIAN_POINT('Ctrl Pts',(0.631684198665438,-0.232861760990032,
0.750785745543687));
#15649=CARTESIAN_POINT('Ctrl Pts',(0.663382628119203,-0.244251601209411,
0.722929908501543));
#15650=CARTESIAN_POINT('Ctrl Pts',(0.679352081686668,-0.246942143572133,
0.707917883896095));
#15651=CARTESIAN_POINT('Ctrl Pts',(0.707917883896095,-0.246942143572133,
0.679352081686668));
#15652=CARTESIAN_POINT('Ctrl Pts',(0.722929908501543,-0.244251601209411,
0.663382628119203));
#15653=CARTESIAN_POINT('Ctrl Pts',(0.750785745543687,-0.232861760990032,
0.631684198665439));
#15654=CARTESIAN_POINT('Ctrl Pts',(0.763642258217232,-0.224161999508995,
0.615966552324775));
#15655=CARTESIAN_POINT('Ctrl Pts',(0.78555112003688,-0.203463743702801,
0.587792702767295));
#15656=CARTESIAN_POINT('Ctrl Pts',(0.795684265985088,-0.190326085855194,
0.573915184558108));
#15657=CARTESIAN_POINT('Ctrl Pts',(0.813159949759,-0.15976606450048,0.548874290046456));
#15658=CARTESIAN_POINT('Ctrl Pts',(0.820511285096538,-0.142345102874864,
0.537715343527944));
#15659=CARTESIAN_POINT('Ctrl Pts',(0.833661031856294,-0.099930567888331,
0.517157748491653));
#15660=CARTESIAN_POINT('Ctrl Pts',(0.838633903678357,-0.0740444353928835,
0.508899795931835));
#15661=CARTESIAN_POINT('Ctrl Pts',(0.841298510752801,-0.0476299999999999,
0.504455939115715));
#15662=CARTESIAN_POINT('',(0.528110872004958,-0.04763,0.871530771444223));
#15663=CARTESIAN_POINT('Origin',(0.707106781186547,-0.04763,0.707106781186548));
#15664=CARTESIAN_POINT('',(0.871530771444223,-0.04763,0.528110872004959));
#15665=CARTESIAN_POINT('Ctrl Pts',(0.871530771444223,-0.0476300000000001,
0.528110872004958));
#15666=CARTESIAN_POINT('Ctrl Pts',(0.87014664509073,-0.0609922781173483,
0.530395067942936));
#15667=CARTESIAN_POINT('Ctrl Pts',(0.868149331745851,-0.0742967091364493,
0.533674141594226));
#15668=CARTESIAN_POINT('Ctrl Pts',(0.85981294420286,-0.115492077056649,
0.54708917182331));
#15669=CARTESIAN_POINT('Ctrl Pts',(0.850993704737257,-0.141695629206859,
0.560922177770136));
#15670=CARTESIAN_POINT('Ctrl Pts',(0.830754510485543,-0.181890537957859,
0.590422647829571));
#15671=CARTESIAN_POINT('Ctrl Pts',(0.816896541396381,-0.201072148666545,
0.609616703125488));
#15672=CARTESIAN_POINT('Ctrl Pts',(0.792310597819928,-0.223955109275652,
0.641117951819998));
#15673=CARTESIAN_POINT('Ctrl Pts',(0.779109323683612,-0.232742381310829,
0.657208095763053));
#15674=CARTESIAN_POINT('Ctrl Pts',(0.750552691816206,-0.244234834628584,
0.68964083160521));
#15675=CARTESIAN_POINT('Ctrl Pts',(0.735185187071673,-0.246942143572133,
0.705971972091755));
#15676=CARTESIAN_POINT('Ctrl Pts',(0.705971972091754,-0.246942143572133,
0.735185187071673));
#15677=CARTESIAN_POINT('Ctrl Pts',(0.689640831605209,-0.244234834628584,
0.750552691816206));
#15678=CARTESIAN_POINT('Ctrl Pts',(0.657208095763052,-0.232742381310829,
0.779109323683612));
#15679=CARTESIAN_POINT('Ctrl Pts',(0.641117951819998,-0.223955109275652,
0.792310597819928));
#15680=CARTESIAN_POINT('Ctrl Pts',(0.609616703125487,-0.201072148666545,
0.816896541396382));
#15681=CARTESIAN_POINT('Ctrl Pts',(0.590422647829571,-0.181890537957858,
0.830754510485544));
#15682=CARTESIAN_POINT('Ctrl Pts',(0.560922177770135,-0.141695629206858,
0.850993704737257));
#15683=CARTESIAN_POINT('Ctrl Pts',(0.547089171823309,-0.115492077056649,
0.859812944202861));
#15684=CARTESIAN_POINT('Ctrl Pts',(0.533674141594226,-0.0742967091364491,
0.868149331745852));
#15685=CARTESIAN_POINT('Ctrl Pts',(0.530395067942936,-0.0609922781173483,
0.870146645090731));
#15686=CARTESIAN_POINT('Ctrl Pts',(0.528110872004958,-0.0476300000000001,
0.871530771444223));
#15687=CARTESIAN_POINT('Origin',(0.707106781186547,-0.04763,0.707106781186548));
#15688=CARTESIAN_POINT('Origin',(0.,-0.166705,0.));
#15689=CARTESIAN_POINT('',(0.242834539687906,-0.04763,0.989696097314));
#15690=CARTESIAN_POINT('Origin',(0.,-0.04763,0.));
#15691=CARTESIAN_POINT('',(-0.242834539687907,-0.04763,0.989696097314));
#15692=CARTESIAN_POINT('Ctrl Pts',(0.242834539687906,-0.04763,0.989696097314));
#15693=CARTESIAN_POINT('Ctrl Pts',(0.24024064412003,-0.0609922781173483,
0.990332542620729));
#15694=CARTESIAN_POINT('Ctrl Pts',(0.236509675094874,-0.0742967091364492,
0.991238884025248));
#15695=CARTESIAN_POINT('Ctrl Pts',(0.221129100087819,-0.115492077056649,
0.994830026707808));
#15696=CARTESIAN_POINT('Ctrl Pts',(0.205111543747588,-0.141695629206859,
0.998375294985966));
#15697=CARTESIAN_POINT('Ctrl Pts',(0.169940289819232,-0.181890537957859,
1.00492400591205));
#15698=CARTESIAN_POINT('Ctrl Pts',(0.1465689792446,-0.201072148666545,1.00869718865384));
#15699=CARTESIAN_POINT('Ctrl Pts',(0.106909345252087,-0.223955109275652,
1.01358704779679));
#15700=CARTESIAN_POINT('Ctrl Pts',(0.0861971848975941,-0.232742381310829,
1.0156297872271));
#15701=CARTESIAN_POINT('Ctrl Pts',(0.0430711894098822,-0.244234834628584,
1.01837060663223));
#15702=CARTESIAN_POINT('Ctrl Pts',(0.0206568624125605,-0.246942143572133,
1.019052));
#15703=CARTESIAN_POINT('Ctrl Pts',(-0.0206568624125608,-0.246942143572133,
1.019052));
#15704=CARTESIAN_POINT('Ctrl Pts',(-0.0430711894098825,-0.244234834628584,
1.01837060663223));
#15705=CARTESIAN_POINT('Ctrl Pts',(-0.0861971848975943,-0.232742381310829,
1.0156297872271));
#15706=CARTESIAN_POINT('Ctrl Pts',(-0.106909345252088,-0.223955109275652,
1.01358704779679));
#15707=CARTESIAN_POINT('Ctrl Pts',(-0.1465689792446,-0.201072148666545,
1.00869718865384));
#15708=CARTESIAN_POINT('Ctrl Pts',(-0.169940289819232,-0.181890537957859,
1.00492400591205));
#15709=CARTESIAN_POINT('Ctrl Pts',(-0.205111543747588,-0.141695629206859,
0.998375294985966));
#15710=CARTESIAN_POINT('Ctrl Pts',(-0.221129100087819,-0.115492077056649,
0.994830026707808));
#15711=CARTESIAN_POINT('Ctrl Pts',(-0.236509675094875,-0.0742967091364493,
0.991238884025248));
#15712=CARTESIAN_POINT('Ctrl Pts',(-0.24024064412003,-0.0609922781173483,
0.990332542620729));
#15713=CARTESIAN_POINT('Ctrl Pts',(-0.242834539687907,-0.04763,0.989696097314));
#15714=CARTESIAN_POINT('',(-0.528110872004959,-0.04763,0.871530771444223));
#15715=CARTESIAN_POINT('Origin',(0.,-0.04763,0.));
#15716=CARTESIAN_POINT('',(-0.871530771444223,-0.04763,0.528110872004958));
#15717=CARTESIAN_POINT('Ctrl Pts',(-0.528110872004958,-0.0476300000000001,
0.871530771444223));
#15718=CARTESIAN_POINT('Ctrl Pts',(-0.530395067942936,-0.0609922781173484,
0.87014664509073));
#15719=CARTESIAN_POINT('Ctrl Pts',(-0.533674141594226,-0.0742967091364493,
0.868149331745851));
#15720=CARTESIAN_POINT('Ctrl Pts',(-0.54708917182331,-0.115492077056649,
0.85981294420286));
#15721=CARTESIAN_POINT('Ctrl Pts',(-0.560922177770136,-0.141695629206859,
0.850993704737257));
#15722=CARTESIAN_POINT('Ctrl Pts',(-0.590422647829571,-0.181890537957859,
0.830754510485543));
#15723=CARTESIAN_POINT('Ctrl Pts',(-0.609616703125488,-0.201072148666545,
0.816896541396381));
#15724=CARTESIAN_POINT('Ctrl Pts',(-0.641117951819998,-0.223955109275652,
0.792310597819928));
#15725=CARTESIAN_POINT('Ctrl Pts',(-0.657208095763053,-0.232742381310829,
0.779109323683611));
#15726=CARTESIAN_POINT('Ctrl Pts',(-0.68964083160521,-0.244234834628584,
0.750552691816205));
#15727=CARTESIAN_POINT('Ctrl Pts',(-0.705971972091755,-0.246942143572133,
0.735185187071673));
#15728=CARTESIAN_POINT('Ctrl Pts',(-0.735185187071673,-0.246942143572133,
0.705971972091754));
#15729=CARTESIAN_POINT('Ctrl Pts',(-0.750552691816206,-0.244234834628584,
0.689640831605209));
#15730=CARTESIAN_POINT('Ctrl Pts',(-0.779109323683612,-0.232742381310829,
0.657208095763052));
#15731=CARTESIAN_POINT('Ctrl Pts',(-0.792310597819928,-0.223955109275652,
0.641117951819998));
#15732=CARTESIAN_POINT('Ctrl Pts',(-0.816896541396382,-0.201072148666545,
0.609616703125487));
#15733=CARTESIAN_POINT('Ctrl Pts',(-0.830754510485544,-0.181890537957858,
0.590422647829571));
#15734=CARTESIAN_POINT('Ctrl Pts',(-0.850993704737257,-0.141695629206858,
0.560922177770135));
#15735=CARTESIAN_POINT('Ctrl Pts',(-0.859812944202861,-0.115492077056649,
0.547089171823309));
#15736=CARTESIAN_POINT('Ctrl Pts',(-0.868149331745852,-0.0742967091364491,
0.533674141594226));
#15737=CARTESIAN_POINT('Ctrl Pts',(-0.870146645090731,-0.0609922781173483,
0.530395067942936));
#15738=CARTESIAN_POINT('Ctrl Pts',(-0.871530771444223,-0.04763,0.528110872004958));
#15739=CARTESIAN_POINT('',(-0.989696097314,-0.04763,0.242834539687906));
#15740=CARTESIAN_POINT('Origin',(0.,-0.04763,0.));
#15741=CARTESIAN_POINT('',(-1.019052,-0.246942143572133,1.248489836334E-16));
#15742=CARTESIAN_POINT('Ctrl Pts',(-0.989696097314,-0.04763,0.242834539687906));
#15743=CARTESIAN_POINT('Ctrl Pts',(-0.990332542620729,-0.0609922781173483,
0.24024064412003));
#15744=CARTESIAN_POINT('Ctrl Pts',(-0.991238884025248,-0.0742967091364492,
0.236509675094874));
#15745=CARTESIAN_POINT('Ctrl Pts',(-0.994830026707808,-0.115492077056649,
0.221129100087819));
#15746=CARTESIAN_POINT('Ctrl Pts',(-0.998375294985966,-0.141695629206859,
0.205111543747588));
#15747=CARTESIAN_POINT('Ctrl Pts',(-1.00492400591205,-0.181890537957859,
0.169940289819232));
#15748=CARTESIAN_POINT('Ctrl Pts',(-1.00869718865384,-0.201072148666545,
0.1465689792446));
#15749=CARTESIAN_POINT('Ctrl Pts',(-1.01358704779679,-0.223955109275652,
0.106909345252088));
#15750=CARTESIAN_POINT('Ctrl Pts',(-1.0156297872271,-0.232742381310829,
0.0861971848975944));
#15751=CARTESIAN_POINT('Ctrl Pts',(-1.01837060663223,-0.244234834628584,
0.0430711894098825));
#15752=CARTESIAN_POINT('Ctrl Pts',(-1.019052,-0.246942143572133,0.0206568624125608));
#15753=CARTESIAN_POINT('Ctrl Pts',(-1.019052,-0.246942143572133,1.2490009027033E-16));
#15754=CARTESIAN_POINT('',(-1.019052,-0.28578,1.24797876996471E-16));
#15755=CARTESIAN_POINT('',(-1.019052,-0.166705,1.24797876996471E-16));
#15756=CARTESIAN_POINT('Origin',(0.,-0.28578,0.));
#15757=CARTESIAN_POINT('',(-0.989696097314,-0.04763,-0.242834539687906));
#15758=CARTESIAN_POINT('Ctrl Pts',(-1.019052,-0.246942143572133,1.2490009027033E-16));
#15759=CARTESIAN_POINT('Ctrl Pts',(-1.019052,-0.246942143572133,-0.0206568624125605));
#15760=CARTESIAN_POINT('Ctrl Pts',(-1.01837060663223,-0.244234834628584,
-0.0430711894098822));
#15761=CARTESIAN_POINT('Ctrl Pts',(-1.0156297872271,-0.232742381310829,
-0.0861971848975941));
#15762=CARTESIAN_POINT('Ctrl Pts',(-1.01358704779679,-0.223955109275652,
-0.106909345252087));
#15763=CARTESIAN_POINT('Ctrl Pts',(-1.00869718865384,-0.201072148666546,
-0.1465689792446));
#15764=CARTESIAN_POINT('Ctrl Pts',(-1.00492400591205,-0.181890537957859,
-0.169940289819232));
#15765=CARTESIAN_POINT('Ctrl Pts',(-0.998375294985966,-0.141695629206859,
-0.205111543747588));
#15766=CARTESIAN_POINT('Ctrl Pts',(-0.994830026707808,-0.11549207705665,
-0.221129100087819));
#15767=CARTESIAN_POINT('Ctrl Pts',(-0.991238884025248,-0.0742967091364495,
-0.236509675094874));
#15768=CARTESIAN_POINT('Ctrl Pts',(-0.990332542620729,-0.0609922781173484,
-0.24024064412003));
#15769=CARTESIAN_POINT('Ctrl Pts',(-0.989696097314,-0.0476300000000001,
-0.242834539687907));
#15770=CARTESIAN_POINT('',(-0.871530771444223,-0.04763,-0.528110872004958));
#15771=CARTESIAN_POINT('Origin',(0.,-0.04763,0.));
#15772=CARTESIAN_POINT('',(-0.528110872004958,-0.04763,-0.871530771444223));
#15773=CARTESIAN_POINT('Ctrl Pts',(-0.871530771444223,-0.0476300000000001,
-0.528110872004958));
#15774=CARTESIAN_POINT('Ctrl Pts',(-0.87014664509073,-0.0609922781173484,
-0.530395067942936));
#15775=CARTESIAN_POINT('Ctrl Pts',(-0.868149331745851,-0.0742967091364494,
-0.533674141594226));
#15776=CARTESIAN_POINT('Ctrl Pts',(-0.85981294420286,-0.115492077056649,
-0.54708917182331));
#15777=CARTESIAN_POINT('Ctrl Pts',(-0.850993704737257,-0.141695629206859,
-0.560922177770136));
#15778=CARTESIAN_POINT('Ctrl Pts',(-0.830754510485543,-0.181890537957859,
-0.590422647829571));
#15779=CARTESIAN_POINT('Ctrl Pts',(-0.816896541396381,-0.201072148666546,
-0.609616703125488));
#15780=CARTESIAN_POINT('Ctrl Pts',(-0.792310597819928,-0.223955109275652,
-0.641117951819999));
#15781=CARTESIAN_POINT('Ctrl Pts',(-0.779109323683611,-0.232742381310829,
-0.657208095763053));
#15782=CARTESIAN_POINT('Ctrl Pts',(-0.750552691816205,-0.244234834628584,
-0.68964083160521));
#15783=CARTESIAN_POINT('Ctrl Pts',(-0.735185187071673,-0.246942143572133,
-0.705971972091755));
#15784=CARTESIAN_POINT('Ctrl Pts',(-0.705971972091754,-0.246942143572133,
-0.735185187071673));
#15785=CARTESIAN_POINT('Ctrl Pts',(-0.68964083160521,-0.244234834628584,
-0.750552691816206));
#15786=CARTESIAN_POINT('Ctrl Pts',(-0.657208095763052,-0.232742381310829,
-0.779109323683612));
#15787=CARTESIAN_POINT('Ctrl Pts',(-0.641117951819998,-0.223955109275652,
-0.792310597819928));
#15788=CARTESIAN_POINT('Ctrl Pts',(-0.609616703125488,-0.201072148666545,
-0.816896541396381));
#15789=CARTESIAN_POINT('Ctrl Pts',(-0.590422647829571,-0.181890537957859,
-0.830754510485543));
#15790=CARTESIAN_POINT('Ctrl Pts',(-0.560922177770136,-0.141695629206859,
-0.850993704737257));
#15791=CARTESIAN_POINT('Ctrl Pts',(-0.54708917182331,-0.115492077056649,
-0.85981294420286));
#15792=CARTESIAN_POINT('Ctrl Pts',(-0.533674141594226,-0.0742967091364494,
-0.868149331745852));
#15793=CARTESIAN_POINT('Ctrl Pts',(-0.530395067942936,-0.0609922781173484,
-0.870146645090731));
#15794=CARTESIAN_POINT('Ctrl Pts',(-0.528110872004958,-0.0476300000000001,
-0.871530771444223));
#15795=CARTESIAN_POINT('',(-0.242834539687906,-0.04763,-0.989696097314));
#15796=CARTESIAN_POINT('Origin',(0.,-0.04763,0.));
#15797=CARTESIAN_POINT('',(0.242834539687906,-0.04763,-0.989696097314));
#15798=CARTESIAN_POINT('Ctrl Pts',(-0.242834539687907,-0.04763,-0.989696097314));
#15799=CARTESIAN_POINT('Ctrl Pts',(-0.24024064412003,-0.0609922781173483,
-0.990332542620729));
#15800=CARTESIAN_POINT('Ctrl Pts',(-0.236509675094874,-0.0742967091364493,
-0.991238884025248));
#15801=CARTESIAN_POINT('Ctrl Pts',(-0.221129100087819,-0.115492077056649,
-0.994830026707808));
#15802=CARTESIAN_POINT('Ctrl Pts',(-0.205111543747588,-0.141695629206859,
-0.998375294985966));
#15803=CARTESIAN_POINT('Ctrl Pts',(-0.169940289819232,-0.181890537957859,
-1.00492400591205));
#15804=CARTESIAN_POINT('Ctrl Pts',(-0.1465689792446,-0.201072148666545,
-1.00869718865384));
#15805=CARTESIAN_POINT('Ctrl Pts',(-0.106909345252087,-0.223955109275652,
-1.01358704779679));
#15806=CARTESIAN_POINT('Ctrl Pts',(-0.0861971848975942,-0.232742381310829,
-1.0156297872271));
#15807=CARTESIAN_POINT('Ctrl Pts',(-0.0430711894098823,-0.244234834628584,
-1.01837060663223));
#15808=CARTESIAN_POINT('Ctrl Pts',(-0.0206568624125606,-0.246942143572133,
-1.019052));
#15809=CARTESIAN_POINT('Ctrl Pts',(0.0206568624125607,-0.246942143572133,
-1.019052));
#15810=CARTESIAN_POINT('Ctrl Pts',(0.0430711894098824,-0.244234834628584,
-1.01837060663223));
#15811=CARTESIAN_POINT('Ctrl Pts',(0.0861971848975943,-0.232742381310829,
-1.0156297872271));
#15812=CARTESIAN_POINT('Ctrl Pts',(0.106909345252088,-0.223955109275652,
-1.01358704779679));
#15813=CARTESIAN_POINT('Ctrl Pts',(0.1465689792446,-0.201072148666545,-1.00869718865384));
#15814=CARTESIAN_POINT('Ctrl Pts',(0.169940289819232,-0.181890537957859,
-1.00492400591205));
#15815=CARTESIAN_POINT('Ctrl Pts',(0.205111543747588,-0.141695629206859,
-0.998375294985966));
#15816=CARTESIAN_POINT('Ctrl Pts',(0.221129100087819,-0.115492077056649,
-0.994830026707808));
#15817=CARTESIAN_POINT('Ctrl Pts',(0.236509675094874,-0.0742967091364493,
-0.991238884025248));
#15818=CARTESIAN_POINT('Ctrl Pts',(0.24024064412003,-0.0609922781173484,
-0.990332542620729));
#15819=CARTESIAN_POINT('Ctrl Pts',(0.242834539687907,-0.04763,-0.989696097314));
#15820=CARTESIAN_POINT('',(0.528110872004958,-0.04763,-0.871530771444223));
#15821=CARTESIAN_POINT('Origin',(0.,-0.04763,0.));
#15822=CARTESIAN_POINT('',(0.871530771444223,-0.04763,-0.528110872004958));
#15823=CARTESIAN_POINT('Ctrl Pts',(0.528110872004958,-0.0476300000000001,
-0.871530771444223));
#15824=CARTESIAN_POINT('Ctrl Pts',(0.530395067942936,-0.0609922781173484,
-0.870146645090731));
#15825=CARTESIAN_POINT('Ctrl Pts',(0.533674141594226,-0.0742967091364493,
-0.868149331745851));
#15826=CARTESIAN_POINT('Ctrl Pts',(0.54708917182331,-0.115492077056649,
-0.85981294420286));
#15827=CARTESIAN_POINT('Ctrl Pts',(0.560922177770136,-0.141695629206859,
-0.850993704737257));
#15828=CARTESIAN_POINT('Ctrl Pts',(0.590422647829571,-0.181890537957859,
-0.830754510485543));
#15829=CARTESIAN_POINT('Ctrl Pts',(0.609616703125488,-0.201072148666545,
-0.816896541396381));
#15830=CARTESIAN_POINT('Ctrl Pts',(0.641117951819998,-0.223955109275652,
-0.792310597819928));
#15831=CARTESIAN_POINT('Ctrl Pts',(0.657208095763053,-0.232742381310829,
-0.779109323683612));
#15832=CARTESIAN_POINT('Ctrl Pts',(0.68964083160521,-0.244234834628584,
-0.750552691816206));
#15833=CARTESIAN_POINT('Ctrl Pts',(0.705971972091755,-0.246942143572133,
-0.735185187071673));
#15834=CARTESIAN_POINT('Ctrl Pts',(0.735185187071673,-0.246942143572133,
-0.705971972091754));
#15835=CARTESIAN_POINT('Ctrl Pts',(0.750552691816206,-0.244234834628584,
-0.68964083160521));
#15836=CARTESIAN_POINT('Ctrl Pts',(0.779109323683612,-0.232742381310829,
-0.657208095763053));
#15837=CARTESIAN_POINT('Ctrl Pts',(0.792310597819928,-0.223955109275652,
-0.641117951819998));
#15838=CARTESIAN_POINT('Ctrl Pts',(0.816896541396381,-0.201072148666545,
-0.609616703125488));
#15839=CARTESIAN_POINT('Ctrl Pts',(0.830754510485543,-0.181890537957859,
-0.590422647829571));
#15840=CARTESIAN_POINT('Ctrl Pts',(0.850993704737257,-0.141695629206859,
-0.560922177770136));
#15841=CARTESIAN_POINT('Ctrl Pts',(0.85981294420286,-0.115492077056649,
-0.54708917182331));
#15842=CARTESIAN_POINT('Ctrl Pts',(0.868149331745851,-0.0742967091364493,
-0.533674141594226));
#15843=CARTESIAN_POINT('Ctrl Pts',(0.870146645090731,-0.0609922781173484,
-0.530395067942936));
#15844=CARTESIAN_POINT('Ctrl Pts',(0.871530771444223,-0.0476300000000001,
-0.528110872004958));
#15845=CARTESIAN_POINT('',(0.989696097314,-0.04763,-0.242834539687906));
#15846=CARTESIAN_POINT('Origin',(0.,-0.04763,0.));
#15847=CARTESIAN_POINT('',(0.989696097314,-0.04763,0.242834539687906));
#15848=CARTESIAN_POINT('Ctrl Pts',(0.989696097314,-0.04763,-0.242834539687907));
#15849=CARTESIAN_POINT('Ctrl Pts',(0.990332542620729,-0.0609922781173483,
-0.24024064412003));
#15850=CARTESIAN_POINT('Ctrl Pts',(0.991238884025248,-0.0742967091364493,
-0.236509675094874));
#15851=CARTESIAN_POINT('Ctrl Pts',(0.994830026707808,-0.115492077056649,
-0.221129100087819));
#15852=CARTESIAN_POINT('Ctrl Pts',(0.998375294985966,-0.141695629206859,
-0.205111543747588));
#15853=CARTESIAN_POINT('Ctrl Pts',(1.00492400591205,-0.181890537957859,
-0.169940289819232));
#15854=CARTESIAN_POINT('Ctrl Pts',(1.00869718865384,-0.201072148666545,
-0.1465689792446));
#15855=CARTESIAN_POINT('Ctrl Pts',(1.01358704779679,-0.223955109275652,
-0.106909345252087));
#15856=CARTESIAN_POINT('Ctrl Pts',(1.0156297872271,-0.232742381310829,-0.0861971848975942));
#15857=CARTESIAN_POINT('Ctrl Pts',(1.01837060663223,-0.244234834628584,
-0.0430711894098823));
#15858=CARTESIAN_POINT('Ctrl Pts',(1.019052,-0.246942143572133,-0.0206568624125607));
#15859=CARTESIAN_POINT('Ctrl Pts',(1.019052,-0.246942143572133,0.0206568624125607));
#15860=CARTESIAN_POINT('Ctrl Pts',(1.01837060663223,-0.244234834628584,
0.0430711894098823));
#15861=CARTESIAN_POINT('Ctrl Pts',(1.0156297872271,-0.232742381310829,0.0861971848975942));
#15862=CARTESIAN_POINT('Ctrl Pts',(1.01358704779679,-0.223955109275652,
0.106909345252087));
#15863=CARTESIAN_POINT('Ctrl Pts',(1.00869718865384,-0.201072148666545,
0.1465689792446));
#15864=CARTESIAN_POINT('Ctrl Pts',(1.00492400591205,-0.181890537957859,
0.169940289819232));
#15865=CARTESIAN_POINT('Ctrl Pts',(0.998375294985966,-0.141695629206859,
0.205111543747588));
#15866=CARTESIAN_POINT('Ctrl Pts',(0.994830026707808,-0.115492077056649,
0.221129100087819));
#15867=CARTESIAN_POINT('Ctrl Pts',(0.991238884025248,-0.0742967091364492,
0.236509675094874));
#15868=CARTESIAN_POINT('Ctrl Pts',(0.990332542620729,-0.0609922781173483,
0.24024064412003));
#15869=CARTESIAN_POINT('Ctrl Pts',(0.989696097314,-0.04763,0.242834539687907));
#15870=CARTESIAN_POINT('Origin',(0.,-0.04763,0.));
#15871=CARTESIAN_POINT('Origin',(0.,-0.04763,0.));
#15872=CARTESIAN_POINT('',(0.238183666596899,-0.04763,0.951592097314));
#15873=CARTESIAN_POINT('Origin',(0.,-0.04763,0.));
#15874=CARTESIAN_POINT('Origin',(-1.94289029309402E-16,-0.04763,1.));
#15875=CARTESIAN_POINT('Origin',(-1.94289029309402E-16,0.,1.));
#15876=CARTESIAN_POINT('',(-0.2381836665969,-0.04763,0.951592097314));
#15877=CARTESIAN_POINT('Ctrl Pts',(-0.238183666596899,-0.0476299999999999,
0.951592097314));
#15878=CARTESIAN_POINT('Ctrl Pts',(-0.233157223576062,-0.0740444353928835,
0.952850216871763));
#15879=CARTESIAN_POINT('Ctrl Pts',(-0.223801617934946,-0.0999305678883309,
0.955173119738174));
#15880=CARTESIAN_POINT('Ctrl Pts',(-0.199966927975188,-0.142345102874864,
0.960411259488514));
#15881=CARTESIAN_POINT('Ctrl Pts',(-0.1868781821531,-0.159766064500479,
0.963103647174702));
#15882=CARTESIAN_POINT('Ctrl Pts',(-0.15681442133453,-0.190326085855194,
0.968453058988463));
#15883=CARTESIAN_POINT('Ctrl Pts',(-0.139836317888043,-0.203463743702801,
0.971100730005489));
#15884=CARTESIAN_POINT('Ctrl Pts',(-0.104422493053067,-0.224161999508995,
0.975530745318961));
#15885=CARTESIAN_POINT('Ctrl Pts',(-0.0842175114474176,-0.232861760990032,
0.977553872336861));
#15886=CARTESIAN_POINT('Ctrl Pts',(-0.0421062857595701,-0.244251601209411,
0.980270995488453));
#15887=CARTESIAN_POINT('Ctrl Pts',(-0.0201990724523197,-0.246942143572133,
0.980948));
#15888=CARTESIAN_POINT('Ctrl Pts',(0.020199072452319,-0.246942143572133,
0.980948));
#15889=CARTESIAN_POINT('Ctrl Pts',(0.0421062857595694,-0.244251601209411,
0.980270995488454));
#15890=CARTESIAN_POINT('Ctrl Pts',(0.0842175114474169,-0.232861760990032,
0.977553872336861));
#15891=CARTESIAN_POINT('Ctrl Pts',(0.104422493053067,-0.224161999508995,
0.975530745318961));
#15892=CARTESIAN_POINT('Ctrl Pts',(0.139836317888042,-0.203463743702801,
0.971100730005489));
#15893=CARTESIAN_POINT('Ctrl Pts',(0.15681442133453,-0.190326085855194,
0.968453058988463));
#15894=CARTESIAN_POINT('Ctrl Pts',(0.1868781821531,-0.15976606450048,0.963103647174702));
#15895=CARTESIAN_POINT('Ctrl Pts',(0.199966927975188,-0.142345102874864,
0.960411259488514));
#15896=CARTESIAN_POINT('Ctrl Pts',(0.223801617934945,-0.0999305678883309,
0.955173119738174));
#15897=CARTESIAN_POINT('Ctrl Pts',(0.233157223576061,-0.0740444353928835,
0.952850216871763));
#15898=CARTESIAN_POINT('Ctrl Pts',(0.238183666596899,-0.0476299999999999,
0.951592097314));
#15899=CARTESIAN_POINT('Origin',(-1.94289029309402E-16,-0.04763,1.));
#15900=CARTESIAN_POINT('Origin',(0.,-0.04763,0.));
#15901=CARTESIAN_POINT('',(-0.504455939115715,-0.04763,0.841298510752802));
#15902=CARTESIAN_POINT('Origin',(0.,-0.04763,0.));
#15903=CARTESIAN_POINT('Origin',(-0.707106781186548,-0.04763,0.707106781186547));
#15904=CARTESIAN_POINT('Origin',(-0.707106781186548,0.,0.707106781186547));
#15905=CARTESIAN_POINT('',(-0.841298510752802,-0.04763,0.504455939115715));
#15906=CARTESIAN_POINT('Ctrl Pts',(-0.841298510752802,-0.04763,0.504455939115715));
#15907=CARTESIAN_POINT('Ctrl Pts',(-0.838633903678357,-0.0740444353928835,
0.508899795931835));
#15908=CARTESIAN_POINT('Ctrl Pts',(-0.833661031856294,-0.0999305678883309,
0.517157748491652));
#15909=CARTESIAN_POINT('Ctrl Pts',(-0.820511285096538,-0.142345102874864,
0.537715343527944));
#15910=CARTESIAN_POINT('Ctrl Pts',(-0.813159949759,-0.159766064500479,0.548874290046456));
#15911=CARTESIAN_POINT('Ctrl Pts',(-0.795684265985089,-0.190326085855194,
0.573915184558107));
#15912=CARTESIAN_POINT('Ctrl Pts',(-0.78555112003688,-0.203463743702801,
0.587792702767295));
#15913=CARTESIAN_POINT('Ctrl Pts',(-0.763642258217233,-0.224161999508995,
0.615966552324775));
#15914=CARTESIAN_POINT('Ctrl Pts',(-0.750785745543687,-0.232861760990032,
0.631684198665438));
#15915=CARTESIAN_POINT('Ctrl Pts',(-0.722929908501543,-0.244251601209411,
0.663382628119203));
#15916=CARTESIAN_POINT('Ctrl Pts',(-0.707917883896095,-0.246942143572133,
0.679352081686668));
#15917=CARTESIAN_POINT('Ctrl Pts',(-0.679352081686668,-0.246942143572133,
0.707917883896095));
#15918=CARTESIAN_POINT('Ctrl Pts',(-0.663382628119203,-0.244251601209411,
0.722929908501544));
#15919=CARTESIAN_POINT('Ctrl Pts',(-0.631684198665438,-0.232861760990031,
0.750785745543687));
#15920=CARTESIAN_POINT('Ctrl Pts',(-0.615966552324775,-0.224161999508995,
0.763642258217233));
#15921=CARTESIAN_POINT('Ctrl Pts',(-0.587792702767295,-0.203463743702801,
0.78555112003688));
#15922=CARTESIAN_POINT('Ctrl Pts',(-0.573915184558107,-0.190326085855194,
0.795684265985088));
#15923=CARTESIAN_POINT('Ctrl Pts',(-0.548874290046456,-0.159766064500479,
0.813159949759));
#15924=CARTESIAN_POINT('Ctrl Pts',(-0.537715343527944,-0.142345102874864,
0.820511285096538));
#15925=CARTESIAN_POINT('Ctrl Pts',(-0.517157748491652,-0.0999305678883309,
0.833661031856294));
#15926=CARTESIAN_POINT('Ctrl Pts',(-0.508899795931835,-0.0740444353928835,
0.838633903678357));
#15927=CARTESIAN_POINT('Ctrl Pts',(-0.504455939115716,-0.04763,0.841298510752801));
#15928=CARTESIAN_POINT('Origin',(-0.707106781186548,-0.04763,0.707106781186547));
#15929=CARTESIAN_POINT('Origin',(0.,-0.04763,0.));
#15930=CARTESIAN_POINT('',(-0.951592097314,-0.04763,0.238183666596899));
#15931=CARTESIAN_POINT('Origin',(0.,-0.04763,0.));
#15932=CARTESIAN_POINT('Origin',(-1.,-0.04763,-1.11022302462516E-16));
#15933=CARTESIAN_POINT('Origin',(-1.,0.,-1.11022302462516E-16));
#15934=CARTESIAN_POINT('',(-0.951592097314,-0.04763,-0.2381836665969));
#15935=CARTESIAN_POINT('',(-0.980948,-0.246942143572133,1.08514323328844E-18));
#15936=CARTESIAN_POINT('Ctrl Pts',(-0.951592097314,-0.04763,-0.238183666596899));
#15937=CARTESIAN_POINT('Ctrl Pts',(-0.952850216871763,-0.0740444353928835,
-0.233157223576062));
#15938=CARTESIAN_POINT('Ctrl Pts',(-0.955173119738174,-0.0999305678883309,
-0.223801617934946));
#15939=CARTESIAN_POINT('Ctrl Pts',(-0.960411259488514,-0.142345102874864,
-0.199966927975188));
#15940=CARTESIAN_POINT('Ctrl Pts',(-0.963103647174702,-0.159766064500479,
-0.1868781821531));
#15941=CARTESIAN_POINT('Ctrl Pts',(-0.968453058988463,-0.190326085855194,
-0.15681442133453));
#15942=CARTESIAN_POINT('Ctrl Pts',(-0.971100730005489,-0.203463743702801,
-0.139836317888043));
#15943=CARTESIAN_POINT('Ctrl Pts',(-0.975530745318961,-0.224161999508995,
-0.104422493053067));
#15944=CARTESIAN_POINT('Ctrl Pts',(-0.977553872336861,-0.232861760990032,
-0.0842175114474175));
#15945=CARTESIAN_POINT('Ctrl Pts',(-0.980270995488453,-0.244251601209411,
-0.0421062857595699));
#15946=CARTESIAN_POINT('Ctrl Pts',(-0.980948,-0.246942143572133,-0.0201990724523195));
#15947=CARTESIAN_POINT('Ctrl Pts',(-0.980948,-0.246942143572133,-1.17961196366423E-16));
#15948=CARTESIAN_POINT('Origin',(-1.,-0.04763,-1.11022302462516E-16));
#15949=CARTESIAN_POINT('Ctrl Pts',(-0.980948,-0.246942143572133,-1.17961196366423E-16));
#15950=CARTESIAN_POINT('Ctrl Pts',(-0.980948,-0.246942143572133,0.0201990724523192));
#15951=CARTESIAN_POINT('Ctrl Pts',(-0.980270995488453,-0.244251601209411,
0.0421062857595695));
#15952=CARTESIAN_POINT('Ctrl Pts',(-0.977553872336861,-0.232861760990032,
0.0842175114474169));
#15953=CARTESIAN_POINT('Ctrl Pts',(-0.975530745318961,-0.224161999508995,
0.104422493053066));
#15954=CARTESIAN_POINT('Ctrl Pts',(-0.971100730005489,-0.203463743702801,
0.139836317888042));
#15955=CARTESIAN_POINT('Ctrl Pts',(-0.968453058988463,-0.190326085855194,
0.15681442133453));
#15956=CARTESIAN_POINT('Ctrl Pts',(-0.963103647174702,-0.15976606450048,
0.1868781821531));
#15957=CARTESIAN_POINT('Ctrl Pts',(-0.960411259488514,-0.142345102874864,
0.199966927975188));
#15958=CARTESIAN_POINT('Ctrl Pts',(-0.955173119738174,-0.099930567888331,
0.223801617934945));
#15959=CARTESIAN_POINT('Ctrl Pts',(-0.952850216871763,-0.0740444353928835,
0.233157223576061));
#15960=CARTESIAN_POINT('Ctrl Pts',(-0.951592097314,-0.04763,0.238183666596899));
#15961=CARTESIAN_POINT('Origin',(0.,-0.04763,0.));
#15962=CARTESIAN_POINT('',(-0.841298510752802,-0.04763,-0.504455939115715));
#15963=CARTESIAN_POINT('Origin',(0.,-0.04763,0.));
#15964=CARTESIAN_POINT('Origin',(-0.707106781186547,-0.04763,-0.707106781186548));
#15965=CARTESIAN_POINT('Origin',(-0.707106781186547,0.,-0.707106781186548));
#15966=CARTESIAN_POINT('',(-0.504455939115715,-0.04763,-0.841298510752802));
#15967=CARTESIAN_POINT('Ctrl Pts',(-0.504455939115715,-0.04763,-0.841298510752802));
#15968=CARTESIAN_POINT('Ctrl Pts',(-0.508899795931835,-0.0740444353928835,
-0.838633903678357));
#15969=CARTESIAN_POINT('Ctrl Pts',(-0.517157748491652,-0.0999305678883309,
-0.833661031856294));
#15970=CARTESIAN_POINT('Ctrl Pts',(-0.537715343527944,-0.142345102874864,
-0.820511285096538));
#15971=CARTESIAN_POINT('Ctrl Pts',(-0.548874290046456,-0.159766064500479,
-0.813159949759));
#15972=CARTESIAN_POINT('Ctrl Pts',(-0.573915184558107,-0.190326085855194,
-0.795684265985089));
#15973=CARTESIAN_POINT('Ctrl Pts',(-0.587792702767295,-0.203463743702801,
-0.78555112003688));
#15974=CARTESIAN_POINT('Ctrl Pts',(-0.615966552324775,-0.224161999508995,
-0.763642258217233));
#15975=CARTESIAN_POINT('Ctrl Pts',(-0.631684198665438,-0.232861760990032,
-0.750785745543687));
#15976=CARTESIAN_POINT('Ctrl Pts',(-0.663382628119203,-0.244251601209411,
-0.722929908501543));
#15977=CARTESIAN_POINT('Ctrl Pts',(-0.679352081686668,-0.246942143572133,
-0.707917883896095));
#15978=CARTESIAN_POINT('Ctrl Pts',(-0.707917883896095,-0.246942143572133,
-0.679352081686668));
#15979=CARTESIAN_POINT('Ctrl Pts',(-0.722929908501543,-0.244251601209411,
-0.663382628119203));
#15980=CARTESIAN_POINT('Ctrl Pts',(-0.750785745543687,-0.232861760990032,
-0.631684198665439));
#15981=CARTESIAN_POINT('Ctrl Pts',(-0.763642258217232,-0.224161999508995,
-0.615966552324775));
#15982=CARTESIAN_POINT('Ctrl Pts',(-0.78555112003688,-0.203463743702801,
-0.587792702767295));
#15983=CARTESIAN_POINT('Ctrl Pts',(-0.795684265985088,-0.190326085855194,
-0.573915184558107));
#15984=CARTESIAN_POINT('Ctrl Pts',(-0.813159949759,-0.15976606450048,-0.548874290046456));
#15985=CARTESIAN_POINT('Ctrl Pts',(-0.820511285096538,-0.142345102874864,
-0.537715343527944));
#15986=CARTESIAN_POINT('Ctrl Pts',(-0.833661031856294,-0.0999305678883311,
-0.517157748491652));
#15987=CARTESIAN_POINT('Ctrl Pts',(-0.838633903678357,-0.0740444353928836,
-0.508899795931835));
#15988=CARTESIAN_POINT('Ctrl Pts',(-0.841298510752801,-0.04763,-0.504455939115715));
#15989=CARTESIAN_POINT('Origin',(-0.707106781186547,-0.04763,-0.707106781186548));
#15990=CARTESIAN_POINT('Origin',(0.,-0.04763,0.));
#15991=CARTESIAN_POINT('',(-0.238183666596899,-0.04763,-0.951592097314));
#15992=CARTESIAN_POINT('Origin',(0.,-0.04763,0.));
#15993=CARTESIAN_POINT('Origin',(5.55111512312578E-17,-0.04763,-1.));
#15994=CARTESIAN_POINT('Origin',(5.55111512312578E-17,0.,-1.));
#15995=CARTESIAN_POINT('',(0.238183666596899,-0.04763,-0.951592097314));
#15996=CARTESIAN_POINT('Ctrl Pts',(0.238183666596899,-0.04763,-0.951592097314));
#15997=CARTESIAN_POINT('Ctrl Pts',(0.233157223576062,-0.0740444353928835,
-0.952850216871763));
#15998=CARTESIAN_POINT('Ctrl Pts',(0.223801617934946,-0.099930567888331,
-0.955173119738174));
#15999=CARTESIAN_POINT('Ctrl Pts',(0.199966927975188,-0.142345102874864,
-0.960411259488514));
#16000=CARTESIAN_POINT('Ctrl Pts',(0.1868781821531,-0.15976606450048,-0.963103647174702));
#16001=CARTESIAN_POINT('Ctrl Pts',(0.15681442133453,-0.190326085855194,
-0.968453058988463));
#16002=CARTESIAN_POINT('Ctrl Pts',(0.139836317888042,-0.203463743702801,
-0.971100730005489));
#16003=CARTESIAN_POINT('Ctrl Pts',(0.104422493053067,-0.224161999508995,
-0.975530745318961));
#16004=CARTESIAN_POINT('Ctrl Pts',(0.0842175114474173,-0.232861760990032,
-0.977553872336861));
#16005=CARTESIAN_POINT('Ctrl Pts',(0.0421062857595698,-0.244251601209411,
-0.980270995488453));
#16006=CARTESIAN_POINT('Ctrl Pts',(0.0201990724523194,-0.246942143572133,
-0.980948));
#16007=CARTESIAN_POINT('Ctrl Pts',(-0.0201990724523193,-0.246942143572133,
-0.980948));
#16008=CARTESIAN_POINT('Ctrl Pts',(-0.0421062857595697,-0.244251601209411,
-0.980270995488453));
#16009=CARTESIAN_POINT('Ctrl Pts',(-0.0842175114474171,-0.232861760990032,
-0.977553872336861));
#16010=CARTESIAN_POINT('Ctrl Pts',(-0.104422493053067,-0.224161999508995,
-0.975530745318961));
#16011=CARTESIAN_POINT('Ctrl Pts',(-0.139836317888042,-0.203463743702801,
-0.971100730005489));
#16012=CARTESIAN_POINT('Ctrl Pts',(-0.15681442133453,-0.190326085855194,
-0.968453058988463));
#16013=CARTESIAN_POINT('Ctrl Pts',(-0.1868781821531,-0.15976606450048,-0.963103647174702));
#16014=CARTESIAN_POINT('Ctrl Pts',(-0.199966927975188,-0.142345102874864,
-0.960411259488514));
#16015=CARTESIAN_POINT('Ctrl Pts',(-0.223801617934945,-0.099930567888331,
-0.955173119738174));
#16016=CARTESIAN_POINT('Ctrl Pts',(-0.233157223576062,-0.0740444353928835,
-0.952850216871763));
#16017=CARTESIAN_POINT('Ctrl Pts',(-0.238183666596899,-0.0476299999999999,
-0.951592097314));
#16018=CARTESIAN_POINT('Origin',(5.55111512312578E-17,-0.04763,-1.));
#16019=CARTESIAN_POINT('Origin',(0.,-0.04763,0.));
#16020=CARTESIAN_POINT('',(0.504455939115715,-0.04763,-0.841298510752802));
#16021=CARTESIAN_POINT('Origin',(0.,-0.04763,0.));
#16022=CARTESIAN_POINT('Origin',(0.707106781186548,-0.04763,-0.707106781186547));
#16023=CARTESIAN_POINT('Origin',(0.707106781186548,0.,-0.707106781186547));
#16024=CARTESIAN_POINT('',(0.841298510752802,-0.04763,-0.504455939115715));
#16025=CARTESIAN_POINT('Ctrl Pts',(0.841298510752802,-0.04763,-0.504455939115715));
#16026=CARTESIAN_POINT('Ctrl Pts',(0.838633903678357,-0.0740444353928835,
-0.508899795931835));
#16027=CARTESIAN_POINT('Ctrl Pts',(0.833661031856294,-0.0999305678883309,
-0.517157748491652));
#16028=CARTESIAN_POINT('Ctrl Pts',(0.820511285096538,-0.142345102874864,
-0.537715343527944));
#16029=CARTESIAN_POINT('Ctrl Pts',(0.813159949759,-0.159766064500479,-0.548874290046456));
#16030=CARTESIAN_POINT('Ctrl Pts',(0.795684265985088,-0.190326085855194,
-0.573915184558107));
#16031=CARTESIAN_POINT('Ctrl Pts',(0.78555112003688,-0.203463743702801,
-0.587792702767295));
#16032=CARTESIAN_POINT('Ctrl Pts',(0.763642258217233,-0.224161999508995,
-0.615966552324775));
#16033=CARTESIAN_POINT('Ctrl Pts',(0.750785745543687,-0.232861760990032,
-0.631684198665438));
#16034=CARTESIAN_POINT('Ctrl Pts',(0.722929908501543,-0.244251601209411,
-0.663382628119203));
#16035=CARTESIAN_POINT('Ctrl Pts',(0.707917883896095,-0.246942143572133,
-0.679352081686668));
#16036=CARTESIAN_POINT('Ctrl Pts',(0.679352081686668,-0.246942143572133,
-0.707917883896095));
#16037=CARTESIAN_POINT('Ctrl Pts',(0.663382628119203,-0.244251601209411,
-0.722929908501543));
#16038=CARTESIAN_POINT('Ctrl Pts',(0.631684198665438,-0.232861760990032,
-0.750785745543687));
#16039=CARTESIAN_POINT('Ctrl Pts',(0.615966552324775,-0.224161999508995,
-0.763642258217232));
#16040=CARTESIAN_POINT('Ctrl Pts',(0.587792702767295,-0.203463743702801,
-0.78555112003688));
#16041=CARTESIAN_POINT('Ctrl Pts',(0.573915184558107,-0.190326085855194,
-0.795684265985088));
#16042=CARTESIAN_POINT('Ctrl Pts',(0.548874290046456,-0.159766064500479,
-0.813159949759));
#16043=CARTESIAN_POINT('Ctrl Pts',(0.537715343527944,-0.142345102874864,
-0.820511285096538));
#16044=CARTESIAN_POINT('Ctrl Pts',(0.517157748491652,-0.099930567888331,
-0.833661031856294));
#16045=CARTESIAN_POINT('Ctrl Pts',(0.508899795931835,-0.0740444353928835,
-0.838633903678357));
#16046=CARTESIAN_POINT('Ctrl Pts',(0.504455939115715,-0.04763,-0.841298510752801));
#16047=CARTESIAN_POINT('Origin',(0.707106781186548,-0.04763,-0.707106781186547));
#16048=CARTESIAN_POINT('Origin',(0.,-0.166705,0.));
#16049=CARTESIAN_POINT('',(-0.980948,-0.28578,1.20131482833E-16));
#16050=CARTESIAN_POINT('Origin',(0.,-0.28578,0.));
#16051=CARTESIAN_POINT('',(-0.980948,-0.166705,1.20131482833E-16));
#16052=CARTESIAN_POINT('',(0.951592097314,-0.04763,0.238183666596899));
#16053=CARTESIAN_POINT('Origin',(0.,-0.04763,0.));
#16054=CARTESIAN_POINT('',(0.951592097314,-0.04763,-0.238183666596899));
#16055=CARTESIAN_POINT('Ctrl Pts',(0.951592097314,-0.04763,0.238183666596899));
#16056=CARTESIAN_POINT('Ctrl Pts',(0.952850216871763,-0.0740444353928835,
0.233157223576062));
#16057=CARTESIAN_POINT('Ctrl Pts',(0.955173119738174,-0.099930567888331,
0.223801617934945));
#16058=CARTESIAN_POINT('Ctrl Pts',(0.960411259488514,-0.142345102874864,
0.199966927975188));
#16059=CARTESIAN_POINT('Ctrl Pts',(0.963103647174702,-0.15976606450048,
0.1868781821531));
#16060=CARTESIAN_POINT('Ctrl Pts',(0.968453058988463,-0.190326085855194,
0.15681442133453));
#16061=CARTESIAN_POINT('Ctrl Pts',(0.971100730005489,-0.203463743702801,
0.139836317888042));
#16062=CARTESIAN_POINT('Ctrl Pts',(0.975530745318961,-0.224161999508995,
0.104422493053067));
#16063=CARTESIAN_POINT('Ctrl Pts',(0.977553872336861,-0.232861760990032,
0.0842175114474172));
#16064=CARTESIAN_POINT('Ctrl Pts',(0.980270995488453,-0.244251601209411,
0.0421062857595697));
#16065=CARTESIAN_POINT('Ctrl Pts',(0.980948,-0.246942143572133,0.0201990724523194));
#16066=CARTESIAN_POINT('Ctrl Pts',(0.980948,-0.246942143572133,-0.0201990724523194));
#16067=CARTESIAN_POINT('Ctrl Pts',(0.980270995488453,-0.244251601209411,
-0.0421062857595697));
#16068=CARTESIAN_POINT('Ctrl Pts',(0.977553872336861,-0.232861760990032,
-0.0842175114474172));
#16069=CARTESIAN_POINT('Ctrl Pts',(0.975530745318961,-0.224161999508995,
-0.104422493053067));
#16070=CARTESIAN_POINT('Ctrl Pts',(0.971100730005489,-0.203463743702801,
-0.139836317888042));
#16071=CARTESIAN_POINT('Ctrl Pts',(0.968453058988463,-0.190326085855194,
-0.15681442133453));
#16072=CARTESIAN_POINT('Ctrl Pts',(0.963103647174702,-0.15976606450048,
-0.1868781821531));
#16073=CARTESIAN_POINT('Ctrl Pts',(0.960411259488514,-0.142345102874864,
-0.199966927975188));
#16074=CARTESIAN_POINT('Ctrl Pts',(0.955173119738174,-0.099930567888331,
-0.223801617934945));
#16075=CARTESIAN_POINT('Ctrl Pts',(0.952850216871763,-0.0740444353928835,
-0.233157223576062));
#16076=CARTESIAN_POINT('Ctrl Pts',(0.951592097314,-0.0476299999999999,-0.238183666596899));
#16077=CARTESIAN_POINT('Origin',(0.,-0.04763,0.));
#16078=CARTESIAN_POINT('Origin',(0.,-0.04763,0.));
#16079=CARTESIAN_POINT('Origin',(1.,-0.04763,0.));
#16080=CARTESIAN_POINT('Origin',(1.,0.,0.));
#16081=CARTESIAN_POINT('Origin',(1.,-0.04763,0.));
#16082=CARTESIAN_POINT('Origin',(0.,-0.28578,0.));
#16083=CARTESIAN_POINT('Origin',(0.,-0.04763,0.));
#16084=CARTESIAN_POINT('',(0.,0.,0.));
#16085=CARTESIAN_POINT('Origin',(1.013815,0.445,0.));
#16086=CARTESIAN_POINT('',(-1.013815,0.445,-1.24156529467757E-16));
#16087=CARTESIAN_POINT('Origin',(0.,0.445,0.));
#16088=CARTESIAN_POINT('',(-0.991185,0.445,-1.21385153761287E-16));
#16089=CARTESIAN_POINT('Origin',(0.,0.445,0.));
#16090=CARTESIAN_POINT('Origin',(0.,0.4075,0.));
#16091=CARTESIAN_POINT('',(-1.013815,0.37,-1.24156529467757E-16));
#16092=CARTESIAN_POINT('Origin',(0.,0.37,0.));
#16093=CARTESIAN_POINT('',(-1.013815,0.4075,-1.24156529467757E-16));
#16094=CARTESIAN_POINT('Origin',(0.991185,0.37,0.));
#16095=CARTESIAN_POINT('',(-0.991185,0.37,-1.21385153761287E-16));
#16096=CARTESIAN_POINT('Origin',(0.,0.37,0.));
#16097=CARTESIAN_POINT('Origin',(0.,0.4075,0.));
#16098=CARTESIAN_POINT('',(-0.991185,0.4075,-1.21385153761287E-16));
#16099=CARTESIAN_POINT('Origin',(1.013815,-0.37,0.));
#16100=CARTESIAN_POINT('',(-1.013815,-0.37,-1.24156529467757E-16));
#16101=CARTESIAN_POINT('Origin',(0.,-0.37,0.));
#16102=CARTESIAN_POINT('',(-0.991185,-0.37,-1.21385153761287E-16));
#16103=CARTESIAN_POINT('Origin',(0.,-0.37,0.));
#16104=CARTESIAN_POINT('Origin',(0.,-0.4075,0.));
#16105=CARTESIAN_POINT('',(-1.013815,-0.445,-1.24156529467757E-16));
#16106=CARTESIAN_POINT('Origin',(0.,-0.445,0.));
#16107=CARTESIAN_POINT('',(-1.013815,-0.4075,-1.24156529467757E-16));
#16108=CARTESIAN_POINT('Origin',(0.991185,-0.445,0.));
#16109=CARTESIAN_POINT('',(-0.991185,-0.445,-1.21385153761287E-16));
#16110=CARTESIAN_POINT('Origin',(0.,-0.445,0.));
#16111=CARTESIAN_POINT('Origin',(0.,-0.4075,0.));
#16112=CARTESIAN_POINT('',(-0.991185,-0.4075,-1.21385153761287E-16));
#16113=CARTESIAN_POINT('',(0.,0.,0.));
#16114=CARTESIAN_POINT('',(0.,0.,0.));
#16115=CARTESIAN_POINT('',(0.,0.,0.));
#16116=CARTESIAN_POINT('',(0.,0.,0.));
#16117=CARTESIAN_POINT('',(0.,0.,0.));
#16118=CARTESIAN_POINT('',(0.,0.,0.));
#16119=CARTESIAN_POINT('',(0.,0.,0.));
#16120=CARTESIAN_POINT('',(0.,0.,0.));
#16121=CARTESIAN_POINT('',(0.,15.,3.5));
#16122=CARTESIAN_POINT('',(0.,0.,0.));
#16123=CARTESIAN_POINT('',(0.,0.,0.));
#16124=CARTESIAN_POINT('',(0.,0.,0.));
#16125=CARTESIAN_POINT('',(0.,15.,3.5));
#16126=CARTESIAN_POINT('',(0.,0.,0.));
#16127=CARTESIAN_POINT('',(0.,0.,0.));
#16128=CARTESIAN_POINT('',(0.,0.,0.));
#16129=CARTESIAN_POINT('',(0.,15.,3.5));
#16130=CARTESIAN_POINT('',(0.,0.,0.));
#16131=CARTESIAN_POINT('',(0.,0.,0.));
#16132=CARTESIAN_POINT('',(0.,0.,0.));
#16133=CARTESIAN_POINT('',(0.,15.,3.5));
#16134=CARTESIAN_POINT('',(0.,0.,0.));
#16135=CARTESIAN_POINT('',(0.,0.,0.));
#16136=CARTESIAN_POINT('',(0.,0.,0.));
#16137=CARTESIAN_POINT('',(0.,0.,0.));
#16138=CARTESIAN_POINT('',(0.,0.,0.));
#16139=CARTESIAN_POINT('',(0.,0.,0.));
#16140=CARTESIAN_POINT('',(0.,0.,0.));
#16141=CARTESIAN_POINT('',(0.,0.,0.));
#16142=CARTESIAN_POINT('',(0.,0.,0.));
#16143=CARTESIAN_POINT('',(0.,0.,0.));
#16144=UNCERTAINTY_MEASURE_WITH_UNIT(LENGTH_MEASURE(0.001),#16282,
'DISTANCE_ACCURACY_VALUE',
'Maximum model space distance between geometric entities at asserted c
onnectivities');
#16145=UNCERTAINTY_MEASURE_WITH_UNIT(LENGTH_MEASURE(0.001),#16282,
'DISTANCE_ACCURACY_VALUE',
'Maximum model space distance between geometric entities at asserted c
onnectivities');
#16146=UNCERTAINTY_MEASURE_WITH_UNIT(LENGTH_MEASURE(0.001),#16282,
'DISTANCE_ACCURACY_VALUE',
'Maximum model space distance between geometric entities at asserted c
onnectivities');
#16147=UNCERTAINTY_MEASURE_WITH_UNIT(LENGTH_MEASURE(0.001),#16282,
'DISTANCE_ACCURACY_VALUE',
'Maximum model space distance between geometric entities at asserted c
onnectivities');
#16148=UNCERTAINTY_MEASURE_WITH_UNIT(LENGTH_MEASURE(0.001),#16282,
'DISTANCE_ACCURACY_VALUE',
'Maximum model space distance between geometric entities at asserted c
onnectivities');
#16149=UNCERTAINTY_MEASURE_WITH_UNIT(LENGTH_MEASURE(0.001),#16282,
'DISTANCE_ACCURACY_VALUE',
'Maximum model space distance between geometric entities at asserted c
onnectivities');
#16150=UNCERTAINTY_MEASURE_WITH_UNIT(LENGTH_MEASURE(0.001),#16282,
'DISTANCE_ACCURACY_VALUE',
'Maximum model space distance between geometric entities at asserted c
onnectivities');
#16151=UNCERTAINTY_MEASURE_WITH_UNIT(LENGTH_MEASURE(0.001),#16282,
'DISTANCE_ACCURACY_VALUE',
'Maximum model space distance between geometric entities at asserted c
onnectivities');
#16152=UNCERTAINTY_MEASURE_WITH_UNIT(LENGTH_MEASURE(0.001),#16282,
'DISTANCE_ACCURACY_VALUE',
'Maximum model space distance between geometric entities at asserted c
onnectivities');
#16153=UNCERTAINTY_MEASURE_WITH_UNIT(LENGTH_MEASURE(0.001),#16282,
'DISTANCE_ACCURACY_VALUE',
'Maximum model space distance between geometric entities at asserted c
onnectivities');
#16154=UNCERTAINTY_MEASURE_WITH_UNIT(LENGTH_MEASURE(0.001),#16282,
'DISTANCE_ACCURACY_VALUE',
'Maximum model space distance between geometric entities at asserted c
onnectivities');
#16155=UNCERTAINTY_MEASURE_WITH_UNIT(LENGTH_MEASURE(0.001),#16282,
'DISTANCE_ACCURACY_VALUE',
'Maximum model space distance between geometric entities at asserted c
onnectivities');
#16156=UNCERTAINTY_MEASURE_WITH_UNIT(LENGTH_MEASURE(0.001),#16282,
'DISTANCE_ACCURACY_VALUE',
'Maximum model space distance between geometric entities at asserted c
onnectivities');
#16157=UNCERTAINTY_MEASURE_WITH_UNIT(LENGTH_MEASURE(0.001),#16282,
'DISTANCE_ACCURACY_VALUE',
'Maximum model space distance between geometric entities at asserted c
onnectivities');
#16158=UNCERTAINTY_MEASURE_WITH_UNIT(LENGTH_MEASURE(0.001),#16282,
'DISTANCE_ACCURACY_VALUE',
'Maximum model space distance between geometric entities at asserted c
onnectivities');
#16159=UNCERTAINTY_MEASURE_WITH_UNIT(LENGTH_MEASURE(0.001),#16282,
'DISTANCE_ACCURACY_VALUE',
'Maximum model space distance between geometric entities at asserted c
onnectivities');
#16160=UNCERTAINTY_MEASURE_WITH_UNIT(LENGTH_MEASURE(0.001),#16282,
'DISTANCE_ACCURACY_VALUE',
'Maximum model space distance between geometric entities at asserted c
onnectivities');
#16161=UNCERTAINTY_MEASURE_WITH_UNIT(LENGTH_MEASURE(0.001),#16282,
'DISTANCE_ACCURACY_VALUE',
'Maximum model space distance between geometric entities at asserted c
onnectivities');
#16162=UNCERTAINTY_MEASURE_WITH_UNIT(LENGTH_MEASURE(0.001),#16282,
'DISTANCE_ACCURACY_VALUE',
'Maximum model space distance between geometric entities at asserted c
onnectivities');
#16163=UNCERTAINTY_MEASURE_WITH_UNIT(LENGTH_MEASURE(0.001),#16282,
'DISTANCE_ACCURACY_VALUE',
'Maximum model space distance between geometric entities at asserted c
onnectivities');
#16164=UNCERTAINTY_MEASURE_WITH_UNIT(LENGTH_MEASURE(0.001),#16282,
'DISTANCE_ACCURACY_VALUE',
'Maximum model space distance between geometric entities at asserted c
onnectivities');
#16165=UNCERTAINTY_MEASURE_WITH_UNIT(LENGTH_MEASURE(0.001),#16282,
'DISTANCE_ACCURACY_VALUE',
'Maximum model space distance between geometric entities at asserted c
onnectivities');
#16166=UNCERTAINTY_MEASURE_WITH_UNIT(LENGTH_MEASURE(0.001),#16282,
'DISTANCE_ACCURACY_VALUE',
'Maximum model space distance between geometric entities at asserted c
onnectivities');
#16167=UNCERTAINTY_MEASURE_WITH_UNIT(LENGTH_MEASURE(0.001),#16282,
'DISTANCE_ACCURACY_VALUE',
'Maximum model space distance between geometric entities at asserted c
onnectivities');
#16168=UNCERTAINTY_MEASURE_WITH_UNIT(LENGTH_MEASURE(0.001),#16282,
'DISTANCE_ACCURACY_VALUE',
'Maximum model space distance between geometric entities at asserted c
onnectivities');
#16169=UNCERTAINTY_MEASURE_WITH_UNIT(LENGTH_MEASURE(0.001),#16282,
'DISTANCE_ACCURACY_VALUE',
'Maximum model space distance between geometric entities at asserted c
onnectivities');
#16170=UNCERTAINTY_MEASURE_WITH_UNIT(LENGTH_MEASURE(0.001),#16282,
'DISTANCE_ACCURACY_VALUE',
'Maximum model space distance between geometric entities at asserted c
onnectivities');
#16171=UNCERTAINTY_MEASURE_WITH_UNIT(LENGTH_MEASURE(0.001),#16282,
'DISTANCE_ACCURACY_VALUE',
'Maximum model space distance between geometric entities at asserted c
onnectivities');
#16172=UNCERTAINTY_MEASURE_WITH_UNIT(LENGTH_MEASURE(0.001),#16282,
'DISTANCE_ACCURACY_VALUE',
'Maximum model space distance between geometric entities at asserted c
onnectivities');
#16173=UNCERTAINTY_MEASURE_WITH_UNIT(LENGTH_MEASURE(0.001),#16282,
'DISTANCE_ACCURACY_VALUE',
'Maximum model space distance between geometric entities at asserted c
onnectivities');
#16174=UNCERTAINTY_MEASURE_WITH_UNIT(LENGTH_MEASURE(0.001),#16282,
'DISTANCE_ACCURACY_VALUE',
'Maximum model space distance between geometric entities at asserted c
onnectivities');
#16175=UNCERTAINTY_MEASURE_WITH_UNIT(LENGTH_MEASURE(0.001),#16282,
'DISTANCE_ACCURACY_VALUE',
'Maximum model space distance between geometric entities at asserted c
onnectivities');
#16176=UNCERTAINTY_MEASURE_WITH_UNIT(LENGTH_MEASURE(0.001),#16282,
'DISTANCE_ACCURACY_VALUE',
'Maximum model space distance between geometric entities at asserted c
onnectivities');
#16177=UNCERTAINTY_MEASURE_WITH_UNIT(LENGTH_MEASURE(0.001),#16282,
'DISTANCE_ACCURACY_VALUE',
'Maximum model space distance between geometric entities at asserted c
onnectivities');
#16178=UNCERTAINTY_MEASURE_WITH_UNIT(LENGTH_MEASURE(0.001),#16282,
'DISTANCE_ACCURACY_VALUE',
'Maximum model space distance between geometric entities at asserted c
onnectivities');
#16179=UNCERTAINTY_MEASURE_WITH_UNIT(LENGTH_MEASURE(0.001),#16282,
'DISTANCE_ACCURACY_VALUE',
'Maximum model space distance between geometric entities at asserted c
onnectivities');
#16180=UNCERTAINTY_MEASURE_WITH_UNIT(LENGTH_MEASURE(0.001),#16282,
'DISTANCE_ACCURACY_VALUE',
'Maximum model space distance between geometric entities at asserted c
onnectivities');
#16181=UNCERTAINTY_MEASURE_WITH_UNIT(LENGTH_MEASURE(0.001),#16282,
'DISTANCE_ACCURACY_VALUE',
'Maximum model space distance between geometric entities at asserted c
onnectivities');
#16182=UNCERTAINTY_MEASURE_WITH_UNIT(LENGTH_MEASURE(0.001),#16282,
'DISTANCE_ACCURACY_VALUE',
'Maximum model space distance between geometric entities at asserted c
onnectivities');
#16183=UNCERTAINTY_MEASURE_WITH_UNIT(LENGTH_MEASURE(0.001),#16282,
'DISTANCE_ACCURACY_VALUE',
'Maximum model space distance between geometric entities at asserted c
onnectivities');
#16184=UNCERTAINTY_MEASURE_WITH_UNIT(LENGTH_MEASURE(0.001),#16282,
'DISTANCE_ACCURACY_VALUE',
'Maximum model space distance between geometric entities at asserted c
onnectivities');
#16185=UNCERTAINTY_MEASURE_WITH_UNIT(LENGTH_MEASURE(0.001),#16282,
'DISTANCE_ACCURACY_VALUE',
'Maximum model space distance between geometric entities at asserted c
onnectivities');
#16186=UNCERTAINTY_MEASURE_WITH_UNIT(LENGTH_MEASURE(0.001),#16282,
'DISTANCE_ACCURACY_VALUE',
'Maximum model space distance between geometric entities at asserted c
onnectivities');
#16187=UNCERTAINTY_MEASURE_WITH_UNIT(LENGTH_MEASURE(0.001),#16282,
'DISTANCE_ACCURACY_VALUE',
'Maximum model space distance between geometric entities at asserted c
onnectivities');
#16188=UNCERTAINTY_MEASURE_WITH_UNIT(LENGTH_MEASURE(0.001),#16282,
'DISTANCE_ACCURACY_VALUE',
'Maximum model space distance between geometric entities at asserted c
onnectivities');
#16189=UNCERTAINTY_MEASURE_WITH_UNIT(LENGTH_MEASURE(0.001),#16282,
'DISTANCE_ACCURACY_VALUE',
'Maximum model space distance between geometric entities at asserted c
onnectivities');
#16190=UNCERTAINTY_MEASURE_WITH_UNIT(LENGTH_MEASURE(0.001),#16282,
'DISTANCE_ACCURACY_VALUE',
'Maximum model space distance between geometric entities at asserted c
onnectivities');
#16191=UNCERTAINTY_MEASURE_WITH_UNIT(LENGTH_MEASURE(0.001),#16282,
'DISTANCE_ACCURACY_VALUE',
'Maximum model space distance between geometric entities at asserted c
onnectivities');
#16192=UNCERTAINTY_MEASURE_WITH_UNIT(LENGTH_MEASURE(0.001),#16282,
'DISTANCE_ACCURACY_VALUE',
'Maximum model space distance between geometric entities at asserted c
onnectivities');
#16193=UNCERTAINTY_MEASURE_WITH_UNIT(LENGTH_MEASURE(0.001),#16282,
'DISTANCE_ACCURACY_VALUE',
'Maximum model space distance between geometric entities at asserted c
onnectivities');
#16194=UNCERTAINTY_MEASURE_WITH_UNIT(LENGTH_MEASURE(0.001),#16282,
'DISTANCE_ACCURACY_VALUE',
'Maximum model space distance between geometric entities at asserted c
onnectivities');
#16195=UNCERTAINTY_MEASURE_WITH_UNIT(LENGTH_MEASURE(0.001),#16282,
'DISTANCE_ACCURACY_VALUE',
'Maximum model space distance between geometric entities at asserted c
onnectivities');
#16196=UNCERTAINTY_MEASURE_WITH_UNIT(LENGTH_MEASURE(0.001),#16282,
'DISTANCE_ACCURACY_VALUE',
'Maximum model space distance between geometric entities at asserted c
onnectivities');
#16197=UNCERTAINTY_MEASURE_WITH_UNIT(LENGTH_MEASURE(0.001),#16282,
'DISTANCE_ACCURACY_VALUE',
'Maximum model space distance between geometric entities at asserted c
onnectivities');
#16198=UNCERTAINTY_MEASURE_WITH_UNIT(LENGTH_MEASURE(0.001),#16282,
'DISTANCE_ACCURACY_VALUE',
'Maximum model space distance between geometric entities at asserted c
onnectivities');
#16199=UNCERTAINTY_MEASURE_WITH_UNIT(LENGTH_MEASURE(0.001),#16282,
'DISTANCE_ACCURACY_VALUE',
'Maximum model space distance between geometric entities at asserted c
onnectivities');
#16200=UNCERTAINTY_MEASURE_WITH_UNIT(LENGTH_MEASURE(0.001),#16282,
'DISTANCE_ACCURACY_VALUE',
'Maximum model space distance between geometric entities at asserted c
onnectivities');
#16201=UNCERTAINTY_MEASURE_WITH_UNIT(LENGTH_MEASURE(0.001),#16282,
'DISTANCE_ACCURACY_VALUE',
'Maximum model space distance between geometric entities at asserted c
onnectivities');
#16202=UNCERTAINTY_MEASURE_WITH_UNIT(LENGTH_MEASURE(0.001),#16282,
'DISTANCE_ACCURACY_VALUE',
'Maximum model space distance between geometric entities at asserted c
onnectivities');
#16203=UNCERTAINTY_MEASURE_WITH_UNIT(LENGTH_MEASURE(0.001),#16282,
'DISTANCE_ACCURACY_VALUE',
'Maximum model space distance between geometric entities at asserted c
onnectivities');
#16204=UNCERTAINTY_MEASURE_WITH_UNIT(LENGTH_MEASURE(0.001),#16282,
'DISTANCE_ACCURACY_VALUE',
'Maximum model space distance between geometric entities at asserted c
onnectivities');
#16205=UNCERTAINTY_MEASURE_WITH_UNIT(LENGTH_MEASURE(0.001),#16282,
'DISTANCE_ACCURACY_VALUE',
'Maximum model space distance between geometric entities at asserted c
onnectivities');
#16206=UNCERTAINTY_MEASURE_WITH_UNIT(LENGTH_MEASURE(0.001),#16282,
'DISTANCE_ACCURACY_VALUE',
'Maximum model space distance between geometric entities at asserted c
onnectivities');
#16207=UNCERTAINTY_MEASURE_WITH_UNIT(LENGTH_MEASURE(0.001),#16282,
'DISTANCE_ACCURACY_VALUE',
'Maximum model space distance between geometric entities at asserted c
onnectivities');
#16208=UNCERTAINTY_MEASURE_WITH_UNIT(LENGTH_MEASURE(0.001),#16282,
'DISTANCE_ACCURACY_VALUE',
'Maximum model space distance between geometric entities at asserted c
onnectivities');
#16209=UNCERTAINTY_MEASURE_WITH_UNIT(LENGTH_MEASURE(0.001),#16282,
'DISTANCE_ACCURACY_VALUE',
'Maximum model space distance between geometric entities at asserted c
onnectivities');
#16210=UNCERTAINTY_MEASURE_WITH_UNIT(LENGTH_MEASURE(0.001),#16282,
'DISTANCE_ACCURACY_VALUE',
'Maximum model space distance between geometric entities at asserted c
onnectivities');
#16211=UNCERTAINTY_MEASURE_WITH_UNIT(LENGTH_MEASURE(0.001),#16282,
'DISTANCE_ACCURACY_VALUE',
'Maximum model space distance between geometric entities at asserted c
onnectivities');
#16212=UNCERTAINTY_MEASURE_WITH_UNIT(LENGTH_MEASURE(0.001),#16282,
'DISTANCE_ACCURACY_VALUE',
'Maximum model space distance between geometric entities at asserted c
onnectivities');
#16213=(
GEOMETRIC_REPRESENTATION_CONTEXT(3)
GLOBAL_UNCERTAINTY_ASSIGNED_CONTEXT((#16144))
GLOBAL_UNIT_ASSIGNED_CONTEXT((#16282,#16284,#16285))
REPRESENTATION_CONTEXT('','3D')
);
#16214=(
GEOMETRIC_REPRESENTATION_CONTEXT(3)
GLOBAL_UNCERTAINTY_ASSIGNED_CONTEXT((#16145))
GLOBAL_UNIT_ASSIGNED_CONTEXT((#16282,#16284,#16285))
REPRESENTATION_CONTEXT('','3D')
);
#16215=(
GEOMETRIC_REPRESENTATION_CONTEXT(3)
GLOBAL_UNCERTAINTY_ASSIGNED_CONTEXT((#16146))
GLOBAL_UNIT_ASSIGNED_CONTEXT((#16282,#16284,#16285))
REPRESENTATION_CONTEXT('','3D')
);
#16216=(
GEOMETRIC_REPRESENTATION_CONTEXT(3)
GLOBAL_UNCERTAINTY_ASSIGNED_CONTEXT((#16147))
GLOBAL_UNIT_ASSIGNED_CONTEXT((#16282,#16284,#16285))
REPRESENTATION_CONTEXT('','3D')
);
#16217=(
GEOMETRIC_REPRESENTATION_CONTEXT(3)
GLOBAL_UNCERTAINTY_ASSIGNED_CONTEXT((#16148))
GLOBAL_UNIT_ASSIGNED_CONTEXT((#16282,#16284,#16285))
REPRESENTATION_CONTEXT('','3D')
);
#16218=(
GEOMETRIC_REPRESENTATION_CONTEXT(3)
GLOBAL_UNCERTAINTY_ASSIGNED_CONTEXT((#16149))
GLOBAL_UNIT_ASSIGNED_CONTEXT((#16282,#16284,#16285))
REPRESENTATION_CONTEXT('','3D')
);
#16219=(
GEOMETRIC_REPRESENTATION_CONTEXT(3)
GLOBAL_UNCERTAINTY_ASSIGNED_CONTEXT((#16150))
GLOBAL_UNIT_ASSIGNED_CONTEXT((#16282,#16284,#16285))
REPRESENTATION_CONTEXT('','3D')
);
#16220=(
GEOMETRIC_REPRESENTATION_CONTEXT(3)
GLOBAL_UNCERTAINTY_ASSIGNED_CONTEXT((#16151))
GLOBAL_UNIT_ASSIGNED_CONTEXT((#16282,#16284,#16285))
REPRESENTATION_CONTEXT('','3D')
);
#16221=(
GEOMETRIC_REPRESENTATION_CONTEXT(3)
GLOBAL_UNCERTAINTY_ASSIGNED_CONTEXT((#16152))
GLOBAL_UNIT_ASSIGNED_CONTEXT((#16282,#16284,#16285))
REPRESENTATION_CONTEXT('','3D')
);
#16222=(
GEOMETRIC_REPRESENTATION_CONTEXT(3)
GLOBAL_UNCERTAINTY_ASSIGNED_CONTEXT((#16153))
GLOBAL_UNIT_ASSIGNED_CONTEXT((#16282,#16284,#16285))
REPRESENTATION_CONTEXT('','3D')
);
#16223=(
GEOMETRIC_REPRESENTATION_CONTEXT(3)
GLOBAL_UNCERTAINTY_ASSIGNED_CONTEXT((#16154))
GLOBAL_UNIT_ASSIGNED_CONTEXT((#16282,#16284,#16285))
REPRESENTATION_CONTEXT('','3D')
);
#16224=(
GEOMETRIC_REPRESENTATION_CONTEXT(3)
GLOBAL_UNCERTAINTY_ASSIGNED_CONTEXT((#16155))
GLOBAL_UNIT_ASSIGNED_CONTEXT((#16282,#16284,#16285))
REPRESENTATION_CONTEXT('','3D')
);
#16225=(
GEOMETRIC_REPRESENTATION_CONTEXT(3)
GLOBAL_UNCERTAINTY_ASSIGNED_CONTEXT((#16156))
GLOBAL_UNIT_ASSIGNED_CONTEXT((#16282,#16284,#16285))
REPRESENTATION_CONTEXT('','3D')
);
#16226=(
GEOMETRIC_REPRESENTATION_CONTEXT(3)
GLOBAL_UNCERTAINTY_ASSIGNED_CONTEXT((#16157))
GLOBAL_UNIT_ASSIGNED_CONTEXT((#16282,#16284,#16285))
REPRESENTATION_CONTEXT('','3D')
);
#16227=(
GEOMETRIC_REPRESENTATION_CONTEXT(3)
GLOBAL_UNCERTAINTY_ASSIGNED_CONTEXT((#16158))
GLOBAL_UNIT_ASSIGNED_CONTEXT((#16282,#16284,#16285))
REPRESENTATION_CONTEXT('','3D')
);
#16228=(
GEOMETRIC_REPRESENTATION_CONTEXT(3)
GLOBAL_UNCERTAINTY_ASSIGNED_CONTEXT((#16159))
GLOBAL_UNIT_ASSIGNED_CONTEXT((#16282,#16284,#16285))
REPRESENTATION_CONTEXT('','3D')
);
#16229=(
GEOMETRIC_REPRESENTATION_CONTEXT(3)
GLOBAL_UNCERTAINTY_ASSIGNED_CONTEXT((#16160))
GLOBAL_UNIT_ASSIGNED_CONTEXT((#16282,#16284,#16285))
REPRESENTATION_CONTEXT('','3D')
);
#16230=(
GEOMETRIC_REPRESENTATION_CONTEXT(3)
GLOBAL_UNCERTAINTY_ASSIGNED_CONTEXT((#16161))
GLOBAL_UNIT_ASSIGNED_CONTEXT((#16282,#16284,#16285))
REPRESENTATION_CONTEXT('','3D')
);
#16231=(
GEOMETRIC_REPRESENTATION_CONTEXT(3)
GLOBAL_UNCERTAINTY_ASSIGNED_CONTEXT((#16162))
GLOBAL_UNIT_ASSIGNED_CONTEXT((#16282,#16284,#16285))
REPRESENTATION_CONTEXT('','3D')
);
#16232=(
GEOMETRIC_REPRESENTATION_CONTEXT(3)
GLOBAL_UNCERTAINTY_ASSIGNED_CONTEXT((#16163))
GLOBAL_UNIT_ASSIGNED_CONTEXT((#16282,#16284,#16285))
REPRESENTATION_CONTEXT('','3D')
);
#16233=(
GEOMETRIC_REPRESENTATION_CONTEXT(3)
GLOBAL_UNCERTAINTY_ASSIGNED_CONTEXT((#16164))
GLOBAL_UNIT_ASSIGNED_CONTEXT((#16282,#16284,#16285))
REPRESENTATION_CONTEXT('','3D')
);
#16234=(
GEOMETRIC_REPRESENTATION_CONTEXT(3)
GLOBAL_UNCERTAINTY_ASSIGNED_CONTEXT((#16165))
GLOBAL_UNIT_ASSIGNED_CONTEXT((#16282,#16284,#16285))
REPRESENTATION_CONTEXT('','3D')
);
#16235=(
GEOMETRIC_REPRESENTATION_CONTEXT(3)
GLOBAL_UNCERTAINTY_ASSIGNED_CONTEXT((#16166))
GLOBAL_UNIT_ASSIGNED_CONTEXT((#16282,#16284,#16285))
REPRESENTATION_CONTEXT('','3D')
);
#16236=(
GEOMETRIC_REPRESENTATION_CONTEXT(3)
GLOBAL_UNCERTAINTY_ASSIGNED_CONTEXT((#16167))
GLOBAL_UNIT_ASSIGNED_CONTEXT((#16282,#16284,#16285))
REPRESENTATION_CONTEXT('','3D')
);
#16237=(
GEOMETRIC_REPRESENTATION_CONTEXT(3)
GLOBAL_UNCERTAINTY_ASSIGNED_CONTEXT((#16168))
GLOBAL_UNIT_ASSIGNED_CONTEXT((#16282,#16284,#16285))
REPRESENTATION_CONTEXT('','3D')
);
#16238=(
GEOMETRIC_REPRESENTATION_CONTEXT(3)
GLOBAL_UNCERTAINTY_ASSIGNED_CONTEXT((#16169))
GLOBAL_UNIT_ASSIGNED_CONTEXT((#16282,#16284,#16285))
REPRESENTATION_CONTEXT('','3D')
);
#16239=(
GEOMETRIC_REPRESENTATION_CONTEXT(3)
GLOBAL_UNCERTAINTY_ASSIGNED_CONTEXT((#16170))
GLOBAL_UNIT_ASSIGNED_CONTEXT((#16282,#16284,#16285))
REPRESENTATION_CONTEXT('','3D')
);
#16240=(
GEOMETRIC_REPRESENTATION_CONTEXT(3)
GLOBAL_UNCERTAINTY_ASSIGNED_CONTEXT((#16171))
GLOBAL_UNIT_ASSIGNED_CONTEXT((#16282,#16284,#16285))
REPRESENTATION_CONTEXT('','3D')
);
#16241=(
GEOMETRIC_REPRESENTATION_CONTEXT(3)
GLOBAL_UNCERTAINTY_ASSIGNED_CONTEXT((#16172))
GLOBAL_UNIT_ASSIGNED_CONTEXT((#16282,#16284,#16285))
REPRESENTATION_CONTEXT('','3D')
);
#16242=(
GEOMETRIC_REPRESENTATION_CONTEXT(3)
GLOBAL_UNCERTAINTY_ASSIGNED_CONTEXT((#16173))
GLOBAL_UNIT_ASSIGNED_CONTEXT((#16282,#16284,#16285))
REPRESENTATION_CONTEXT('','3D')
);
#16243=(
GEOMETRIC_REPRESENTATION_CONTEXT(3)
GLOBAL_UNCERTAINTY_ASSIGNED_CONTEXT((#16174))
GLOBAL_UNIT_ASSIGNED_CONTEXT((#16282,#16284,#16285))
REPRESENTATION_CONTEXT('','3D')
);
#16244=(
GEOMETRIC_REPRESENTATION_CONTEXT(3)
GLOBAL_UNCERTAINTY_ASSIGNED_CONTEXT((#16175))
GLOBAL_UNIT_ASSIGNED_CONTEXT((#16282,#16284,#16285))
REPRESENTATION_CONTEXT('','3D')
);
#16245=(
GEOMETRIC_REPRESENTATION_CONTEXT(3)
GLOBAL_UNCERTAINTY_ASSIGNED_CONTEXT((#16176))
GLOBAL_UNIT_ASSIGNED_CONTEXT((#16282,#16284,#16285))
REPRESENTATION_CONTEXT('','3D')
);
#16246=(
GEOMETRIC_REPRESENTATION_CONTEXT(3)
GLOBAL_UNCERTAINTY_ASSIGNED_CONTEXT((#16177))
GLOBAL_UNIT_ASSIGNED_CONTEXT((#16282,#16284,#16285))
REPRESENTATION_CONTEXT('','3D')
);
#16247=(
GEOMETRIC_REPRESENTATION_CONTEXT(3)
GLOBAL_UNCERTAINTY_ASSIGNED_CONTEXT((#16178))
GLOBAL_UNIT_ASSIGNED_CONTEXT((#16282,#16284,#16285))
REPRESENTATION_CONTEXT('','3D')
);
#16248=(
GEOMETRIC_REPRESENTATION_CONTEXT(3)
GLOBAL_UNCERTAINTY_ASSIGNED_CONTEXT((#16179))
GLOBAL_UNIT_ASSIGNED_CONTEXT((#16282,#16284,#16285))
REPRESENTATION_CONTEXT('','3D')
);
#16249=(
GEOMETRIC_REPRESENTATION_CONTEXT(3)
GLOBAL_UNCERTAINTY_ASSIGNED_CONTEXT((#16180))
GLOBAL_UNIT_ASSIGNED_CONTEXT((#16282,#16284,#16285))
REPRESENTATION_CONTEXT('','3D')
);
#16250=(
GEOMETRIC_REPRESENTATION_CONTEXT(3)
GLOBAL_UNCERTAINTY_ASSIGNED_CONTEXT((#16181))
GLOBAL_UNIT_ASSIGNED_CONTEXT((#16282,#16284,#16285))
REPRESENTATION_CONTEXT('','3D')
);
#16251=(
GEOMETRIC_REPRESENTATION_CONTEXT(3)
GLOBAL_UNCERTAINTY_ASSIGNED_CONTEXT((#16182))
GLOBAL_UNIT_ASSIGNED_CONTEXT((#16282,#16284,#16285))
REPRESENTATION_CONTEXT('','3D')
);
#16252=(
GEOMETRIC_REPRESENTATION_CONTEXT(3)
GLOBAL_UNCERTAINTY_ASSIGNED_CONTEXT((#16183))
GLOBAL_UNIT_ASSIGNED_CONTEXT((#16282,#16284,#16285))
REPRESENTATION_CONTEXT('','3D')
);
#16253=(
GEOMETRIC_REPRESENTATION_CONTEXT(3)
GLOBAL_UNCERTAINTY_ASSIGNED_CONTEXT((#16184))
GLOBAL_UNIT_ASSIGNED_CONTEXT((#16282,#16284,#16285))
REPRESENTATION_CONTEXT('','3D')
);
#16254=(
GEOMETRIC_REPRESENTATION_CONTEXT(3)
GLOBAL_UNCERTAINTY_ASSIGNED_CONTEXT((#16185))
GLOBAL_UNIT_ASSIGNED_CONTEXT((#16282,#16284,#16285))
REPRESENTATION_CONTEXT('','3D')
);
#16255=(
GEOMETRIC_REPRESENTATION_CONTEXT(3)
GLOBAL_UNCERTAINTY_ASSIGNED_CONTEXT((#16186))
GLOBAL_UNIT_ASSIGNED_CONTEXT((#16282,#16284,#16285))
REPRESENTATION_CONTEXT('','3D')
);
#16256=(
GEOMETRIC_REPRESENTATION_CONTEXT(3)
GLOBAL_UNCERTAINTY_ASSIGNED_CONTEXT((#16187))
GLOBAL_UNIT_ASSIGNED_CONTEXT((#16282,#16284,#16285))
REPRESENTATION_CONTEXT('','3D')
);
#16257=(
GEOMETRIC_REPRESENTATION_CONTEXT(3)
GLOBAL_UNCERTAINTY_ASSIGNED_CONTEXT((#16188))
GLOBAL_UNIT_ASSIGNED_CONTEXT((#16282,#16284,#16285))
REPRESENTATION_CONTEXT('','3D')
);
#16258=(
GEOMETRIC_REPRESENTATION_CONTEXT(3)
GLOBAL_UNCERTAINTY_ASSIGNED_CONTEXT((#16189))
GLOBAL_UNIT_ASSIGNED_CONTEXT((#16282,#16284,#16285))
REPRESENTATION_CONTEXT('','3D')
);
#16259=(
GEOMETRIC_REPRESENTATION_CONTEXT(3)
GLOBAL_UNCERTAINTY_ASSIGNED_CONTEXT((#16190))
GLOBAL_UNIT_ASSIGNED_CONTEXT((#16282,#16284,#16285))
REPRESENTATION_CONTEXT('','3D')
);
#16260=(
GEOMETRIC_REPRESENTATION_CONTEXT(3)
GLOBAL_UNCERTAINTY_ASSIGNED_CONTEXT((#16191))
GLOBAL_UNIT_ASSIGNED_CONTEXT((#16282,#16284,#16285))
REPRESENTATION_CONTEXT('','3D')
);
#16261=(
GEOMETRIC_REPRESENTATION_CONTEXT(3)
GLOBAL_UNCERTAINTY_ASSIGNED_CONTEXT((#16192))
GLOBAL_UNIT_ASSIGNED_CONTEXT((#16282,#16284,#16285))
REPRESENTATION_CONTEXT('','3D')
);
#16262=(
GEOMETRIC_REPRESENTATION_CONTEXT(3)
GLOBAL_UNCERTAINTY_ASSIGNED_CONTEXT((#16193))
GLOBAL_UNIT_ASSIGNED_CONTEXT((#16282,#16284,#16285))
REPRESENTATION_CONTEXT('','3D')
);
#16263=(
GEOMETRIC_REPRESENTATION_CONTEXT(3)
GLOBAL_UNCERTAINTY_ASSIGNED_CONTEXT((#16194))
GLOBAL_UNIT_ASSIGNED_CONTEXT((#16282,#16284,#16285))
REPRESENTATION_CONTEXT('','3D')
);
#16264=(
GEOMETRIC_REPRESENTATION_CONTEXT(3)
GLOBAL_UNCERTAINTY_ASSIGNED_CONTEXT((#16195))
GLOBAL_UNIT_ASSIGNED_CONTEXT((#16282,#16284,#16285))
REPRESENTATION_CONTEXT('','3D')
);
#16265=(
GEOMETRIC_REPRESENTATION_CONTEXT(3)
GLOBAL_UNCERTAINTY_ASSIGNED_CONTEXT((#16196))
GLOBAL_UNIT_ASSIGNED_CONTEXT((#16282,#16284,#16285))
REPRESENTATION_CONTEXT('','3D')
);
#16266=(
GEOMETRIC_REPRESENTATION_CONTEXT(3)
GLOBAL_UNCERTAINTY_ASSIGNED_CONTEXT((#16197))
GLOBAL_UNIT_ASSIGNED_CONTEXT((#16282,#16284,#16285))
REPRESENTATION_CONTEXT('','3D')
);
#16267=(
GEOMETRIC_REPRESENTATION_CONTEXT(3)
GLOBAL_UNCERTAINTY_ASSIGNED_CONTEXT((#16198))
GLOBAL_UNIT_ASSIGNED_CONTEXT((#16282,#16284,#16285))
REPRESENTATION_CONTEXT('','3D')
);
#16268=(
GEOMETRIC_REPRESENTATION_CONTEXT(3)
GLOBAL_UNCERTAINTY_ASSIGNED_CONTEXT((#16199))
GLOBAL_UNIT_ASSIGNED_CONTEXT((#16282,#16284,#16285))
REPRESENTATION_CONTEXT('','3D')
);
#16269=(
GEOMETRIC_REPRESENTATION_CONTEXT(3)
GLOBAL_UNCERTAINTY_ASSIGNED_CONTEXT((#16200))
GLOBAL_UNIT_ASSIGNED_CONTEXT((#16282,#16284,#16285))
REPRESENTATION_CONTEXT('','3D')
);
#16270=(
GEOMETRIC_REPRESENTATION_CONTEXT(3)
GLOBAL_UNCERTAINTY_ASSIGNED_CONTEXT((#16201))
GLOBAL_UNIT_ASSIGNED_CONTEXT((#16282,#16284,#16285))
REPRESENTATION_CONTEXT('','3D')
);
#16271=(
GEOMETRIC_REPRESENTATION_CONTEXT(3)
GLOBAL_UNCERTAINTY_ASSIGNED_CONTEXT((#16202))
GLOBAL_UNIT_ASSIGNED_CONTEXT((#16282,#16284,#16285))
REPRESENTATION_CONTEXT('','3D')
);
#16272=(
GEOMETRIC_REPRESENTATION_CONTEXT(3)
GLOBAL_UNCERTAINTY_ASSIGNED_CONTEXT((#16203))
GLOBAL_UNIT_ASSIGNED_CONTEXT((#16282,#16284,#16285))
REPRESENTATION_CONTEXT('','3D')
);
#16273=(
GEOMETRIC_REPRESENTATION_CONTEXT(3)
GLOBAL_UNCERTAINTY_ASSIGNED_CONTEXT((#16204))
GLOBAL_UNIT_ASSIGNED_CONTEXT((#16282,#16284,#16285))
REPRESENTATION_CONTEXT('','3D')
);
#16274=(
GEOMETRIC_REPRESENTATION_CONTEXT(3)
GLOBAL_UNCERTAINTY_ASSIGNED_CONTEXT((#16205))
GLOBAL_UNIT_ASSIGNED_CONTEXT((#16282,#16284,#16285))
REPRESENTATION_CONTEXT('','3D')
);
#16275=(
GEOMETRIC_REPRESENTATION_CONTEXT(3)
GLOBAL_UNCERTAINTY_ASSIGNED_CONTEXT((#16206))
GLOBAL_UNIT_ASSIGNED_CONTEXT((#16282,#16284,#16285))
REPRESENTATION_CONTEXT('','3D')
);
#16276=(
GEOMETRIC_REPRESENTATION_CONTEXT(3)
GLOBAL_UNCERTAINTY_ASSIGNED_CONTEXT((#16207))
GLOBAL_UNIT_ASSIGNED_CONTEXT((#16282,#16284,#16285))
REPRESENTATION_CONTEXT('','3D')
);
#16277=(
GEOMETRIC_REPRESENTATION_CONTEXT(3)
GLOBAL_UNCERTAINTY_ASSIGNED_CONTEXT((#16208))
GLOBAL_UNIT_ASSIGNED_CONTEXT((#16282,#16284,#16285))
REPRESENTATION_CONTEXT('','3D')
);
#16278=(
GEOMETRIC_REPRESENTATION_CONTEXT(3)
GLOBAL_UNCERTAINTY_ASSIGNED_CONTEXT((#16209))
GLOBAL_UNIT_ASSIGNED_CONTEXT((#16282,#16284,#16285))
REPRESENTATION_CONTEXT('','3D')
);
#16279=(
GEOMETRIC_REPRESENTATION_CONTEXT(3)
GLOBAL_UNCERTAINTY_ASSIGNED_CONTEXT((#16210))
GLOBAL_UNIT_ASSIGNED_CONTEXT((#16282,#16284,#16285))
REPRESENTATION_CONTEXT('','3D')
);
#16280=(
GEOMETRIC_REPRESENTATION_CONTEXT(3)
GLOBAL_UNCERTAINTY_ASSIGNED_CONTEXT((#16211))
GLOBAL_UNIT_ASSIGNED_CONTEXT((#16282,#16284,#16285))
REPRESENTATION_CONTEXT('','3D')
);
#16281=(
GEOMETRIC_REPRESENTATION_CONTEXT(3)
GLOBAL_UNCERTAINTY_ASSIGNED_CONTEXT((#16212))
GLOBAL_UNIT_ASSIGNED_CONTEXT((#16282,#16284,#16285))
REPRESENTATION_CONTEXT('','3D')
);
#16282=(
LENGTH_UNIT()
NAMED_UNIT(*)
SI_UNIT(.CENTI.,.METRE.)
);
#16283=(
LENGTH_UNIT()
NAMED_UNIT(*)
SI_UNIT($,.METRE.)
);
#16284=(
NAMED_UNIT(*)
PLANE_ANGLE_UNIT()
SI_UNIT($,.RADIAN.)
);
#16285=(
NAMED_UNIT(*)
SI_UNIT($,.STERADIAN.)
SOLID_ANGLE_UNIT()
);
#16286=SHAPE_DEFINITION_REPRESENTATION(#16354,#16519);
#16287=SHAPE_DEFINITION_REPRESENTATION(#16355,#16520);
#16288=SHAPE_DEFINITION_REPRESENTATION(#16356,#16521);
#16289=SHAPE_DEFINITION_REPRESENTATION(#16357,#16522);
#16290=SHAPE_DEFINITION_REPRESENTATION(#16358,#16523);
#16291=SHAPE_DEFINITION_REPRESENTATION(#16359,#16524);
#16292=SHAPE_DEFINITION_REPRESENTATION(#16360,#16525);
#16293=SHAPE_DEFINITION_REPRESENTATION(#16361,#16526);
#16294=SHAPE_DEFINITION_REPRESENTATION(#16362,#16527);
#16295=SHAPE_DEFINITION_REPRESENTATION(#16363,#16528);
#16296=SHAPE_DEFINITION_REPRESENTATION(#16364,#16529);
#16297=SHAPE_DEFINITION_REPRESENTATION(#16365,#16530);
#16298=SHAPE_DEFINITION_REPRESENTATION(#16371,#16531);
#16299=SHAPE_DEFINITION_REPRESENTATION(#16372,#16532);
#16300=SHAPE_DEFINITION_REPRESENTATION(#16373,#16533);
#16301=SHAPE_DEFINITION_REPRESENTATION(#16374,#16534);
#16302=SHAPE_DEFINITION_REPRESENTATION(#16375,#16535);
#16303=SHAPE_DEFINITION_REPRESENTATION(#16376,#16536);
#16304=SHAPE_DEFINITION_REPRESENTATION(#16377,#16537);
#16305=SHAPE_DEFINITION_REPRESENTATION(#16392,#16538);
#16306=SHAPE_DEFINITION_REPRESENTATION(#16400,#16539);
#16307=SHAPE_DEFINITION_REPRESENTATION(#16401,#16540);
#16308=SHAPE_DEFINITION_REPRESENTATION(#16402,#16541);
#16309=SHAPE_DEFINITION_REPRESENTATION(#16403,#16542);
#16310=SHAPE_DEFINITION_REPRESENTATION(#16404,#16543);
#16311=SHAPE_DEFINITION_REPRESENTATION(#16405,#16544);
#16312=SHAPE_DEFINITION_REPRESENTATION(#16406,#16545);
#16313=SHAPE_DEFINITION_REPRESENTATION(#16407,#16546);
#16314=SHAPE_DEFINITION_REPRESENTATION(#16408,#16547);
#16315=SHAPE_DEFINITION_REPRESENTATION(#16409,#16548);
#16316=SHAPE_DEFINITION_REPRESENTATION(#16410,#16549);
#16317=SHAPE_DEFINITION_REPRESENTATION(#16411,#16550);
#16318=SHAPE_DEFINITION_REPRESENTATION(#16412,#16551);
#16319=SHAPE_DEFINITION_REPRESENTATION(#16413,#16552);
#16320=SHAPE_DEFINITION_REPRESENTATION(#16414,#16553);
#16321=SHAPE_DEFINITION_REPRESENTATION(#16415,#16554);
#16322=SHAPE_DEFINITION_REPRESENTATION(#16416,#16555);
#16323=SHAPE_DEFINITION_REPRESENTATION(#16417,#16556);
#16324=SHAPE_DEFINITION_REPRESENTATION(#16418,#16557);
#16325=SHAPE_DEFINITION_REPRESENTATION(#16419,#16558);
#16326=SHAPE_DEFINITION_REPRESENTATION(#16420,#16559);
#16327=SHAPE_DEFINITION_REPRESENTATION(#16421,#16560);
#16328=SHAPE_DEFINITION_REPRESENTATION(#16422,#16561);
#16329=SHAPE_DEFINITION_REPRESENTATION(#16423,#16562);
#16330=SHAPE_DEFINITION_REPRESENTATION(#16424,#16563);
#16331=SHAPE_DEFINITION_REPRESENTATION(#16425,#16564);
#16332=SHAPE_DEFINITION_REPRESENTATION(#16466,#16565);
#16333=SHAPE_DEFINITION_REPRESENTATION(#16467,#16566);
#16334=SHAPE_DEFINITION_REPRESENTATION(#16468,#16567);
#16335=SHAPE_DEFINITION_REPRESENTATION(#16469,#16568);
#16336=SHAPE_DEFINITION_REPRESENTATION(#16470,#16569);
#16337=SHAPE_DEFINITION_REPRESENTATION(#16471,#16570);
#16338=SHAPE_DEFINITION_REPRESENTATION(#16472,#16571);
#16339=SHAPE_DEFINITION_REPRESENTATION(#16473,#16572);
#16340=SHAPE_DEFINITION_REPRESENTATION(#16474,#16573);
#16341=SHAPE_DEFINITION_REPRESENTATION(#16475,#16574);
#16342=SHAPE_DEFINITION_REPRESENTATION(#16476,#16575);
#16343=SHAPE_DEFINITION_REPRESENTATION(#16477,#16576);
#16344=SHAPE_DEFINITION_REPRESENTATION(#16478,#16577);
#16345=SHAPE_DEFINITION_REPRESENTATION(#16479,#16578);
#16346=SHAPE_DEFINITION_REPRESENTATION(#16480,#16579);
#16347=SHAPE_DEFINITION_REPRESENTATION(#16481,#16580);
#16348=SHAPE_DEFINITION_REPRESENTATION(#16482,#16581);
#16349=SHAPE_DEFINITION_REPRESENTATION(#16483,#16582);
#16350=SHAPE_DEFINITION_REPRESENTATION(#16484,#16583);
#16351=SHAPE_DEFINITION_REPRESENTATION(#16485,#16584);
#16352=SHAPE_DEFINITION_REPRESENTATION(#16486,#16585);
#16353=SHAPE_DEFINITION_REPRESENTATION(#16487,#16586);
#16354=PRODUCT_DEFINITION_SHAPE('',$,#16588);
#16355=PRODUCT_DEFINITION_SHAPE('',$,#16589);
#16356=PRODUCT_DEFINITION_SHAPE('',$,#16590);
#16357=PRODUCT_DEFINITION_SHAPE('',$,#16591);
#16358=PRODUCT_DEFINITION_SHAPE('',$,#16592);
#16359=PRODUCT_DEFINITION_SHAPE('',$,#16593);
#16360=PRODUCT_DEFINITION_SHAPE('',$,#16594);
#16361=PRODUCT_DEFINITION_SHAPE('',$,#16595);
#16362=PRODUCT_DEFINITION_SHAPE('',$,#16596);
#16363=PRODUCT_DEFINITION_SHAPE('',$,#16597);
#16364=PRODUCT_DEFINITION_SHAPE('',$,#16598);
#16365=PRODUCT_DEFINITION_SHAPE('',$,#16599);
#16366=PRODUCT_DEFINITION_SHAPE($,$,#302);
#16367=PRODUCT_DEFINITION_SHAPE($,$,#303);
#16368=PRODUCT_DEFINITION_SHAPE($,$,#304);
#16369=PRODUCT_DEFINITION_SHAPE($,$,#305);
#16370=PRODUCT_DEFINITION_SHAPE($,$,#306);
#16371=PRODUCT_DEFINITION_SHAPE('',$,#16600);
#16372=PRODUCT_DEFINITION_SHAPE('',$,#16601);
#16373=PRODUCT_DEFINITION_SHAPE('',$,#16602);
#16374=PRODUCT_DEFINITION_SHAPE('',$,#16603);
#16375=PRODUCT_DEFINITION_SHAPE('',$,#16604);
#16376=PRODUCT_DEFINITION_SHAPE('',$,#16605);
#16377=PRODUCT_DEFINITION_SHAPE('',$,#16606);
#16378=PRODUCT_DEFINITION_SHAPE($,$,#307);
#16379=PRODUCT_DEFINITION_SHAPE($,$,#308);
#16380=PRODUCT_DEFINITION_SHAPE($,$,#309);
#16381=PRODUCT_DEFINITION_SHAPE($,$,#310);
#16382=PRODUCT_DEFINITION_SHAPE($,$,#311);
#16383=PRODUCT_DEFINITION_SHAPE($,$,#312);
#16384=PRODUCT_DEFINITION_SHAPE($,$,#313);
#16385=PRODUCT_DEFINITION_SHAPE($,$,#314);
#16386=PRODUCT_DEFINITION_SHAPE($,$,#315);
#16387=PRODUCT_DEFINITION_SHAPE($,$,#316);
#16388=PRODUCT_DEFINITION_SHAPE($,$,#317);
#16389=PRODUCT_DEFINITION_SHAPE($,$,#318);
#16390=PRODUCT_DEFINITION_SHAPE($,$,#319);
#16391=PRODUCT_DEFINITION_SHAPE($,$,#320);
#16392=PRODUCT_DEFINITION_SHAPE('',$,#16607);
#16393=PRODUCT_DEFINITION_SHAPE($,$,#321);
#16394=PRODUCT_DEFINITION_SHAPE($,$,#322);
#16395=PRODUCT_DEFINITION_SHAPE($,$,#323);
#16396=PRODUCT_DEFINITION_SHAPE($,$,#324);
#16397=PRODUCT_DEFINITION_SHAPE($,$,#325);
#16398=PRODUCT_DEFINITION_SHAPE($,$,#326);
#16399=PRODUCT_DEFINITION_SHAPE($,$,#327);
#16400=PRODUCT_DEFINITION_SHAPE('',$,#16608);
#16401=PRODUCT_DEFINITION_SHAPE('',$,#16609);
#16402=PRODUCT_DEFINITION_SHAPE('',$,#16610);
#16403=PRODUCT_DEFINITION_SHAPE('',$,#16611);
#16404=PRODUCT_DEFINITION_SHAPE('',$,#16612);
#16405=PRODUCT_DEFINITION_SHAPE('',$,#16613);
#16406=PRODUCT_DEFINITION_SHAPE('',$,#16614);
#16407=PRODUCT_DEFINITION_SHAPE('',$,#16615);
#16408=PRODUCT_DEFINITION_SHAPE('',$,#16616);
#16409=PRODUCT_DEFINITION_SHAPE('',$,#16617);
#16410=PRODUCT_DEFINITION_SHAPE('',$,#16618);
#16411=PRODUCT_DEFINITION_SHAPE('',$,#16619);
#16412=PRODUCT_DEFINITION_SHAPE('',$,#16620);
#16413=PRODUCT_DEFINITION_SHAPE('',$,#16621);
#16414=PRODUCT_DEFINITION_SHAPE('',$,#16622);
#16415=PRODUCT_DEFINITION_SHAPE('',$,#16623);
#16416=PRODUCT_DEFINITION_SHAPE('',$,#16624);
#16417=PRODUCT_DEFINITION_SHAPE('',$,#16625);
#16418=PRODUCT_DEFINITION_SHAPE('',$,#16626);
#16419=PRODUCT_DEFINITION_SHAPE('',$,#16627);
#16420=PRODUCT_DEFINITION_SHAPE('',$,#16628);
#16421=PRODUCT_DEFINITION_SHAPE('',$,#16629);
#16422=PRODUCT_DEFINITION_SHAPE('',$,#16630);
#16423=PRODUCT_DEFINITION_SHAPE('',$,#16631);
#16424=PRODUCT_DEFINITION_SHAPE('',$,#16632);
#16425=PRODUCT_DEFINITION_SHAPE('',$,#16633);
#16426=PRODUCT_DEFINITION_SHAPE($,$,#328);
#16427=PRODUCT_DEFINITION_SHAPE($,$,#329);
#16428=PRODUCT_DEFINITION_SHAPE($,$,#330);
#16429=PRODUCT_DEFINITION_SHAPE($,$,#331);
#16430=PRODUCT_DEFINITION_SHAPE($,$,#332);
#16431=PRODUCT_DEFINITION_SHAPE($,$,#333);
#16432=PRODUCT_DEFINITION_SHAPE($,$,#334);
#16433=PRODUCT_DEFINITION_SHAPE($,$,#335);
#16434=PRODUCT_DEFINITION_SHAPE($,$,#336);
#16435=PRODUCT_DEFINITION_SHAPE($,$,#337);
#16436=PRODUCT_DEFINITION_SHAPE($,$,#338);
#16437=PRODUCT_DEFINITION_SHAPE($,$,#339);
#16438=PRODUCT_DEFINITION_SHAPE($,$,#340);
#16439=PRODUCT_DEFINITION_SHAPE($,$,#341);
#16440=PRODUCT_DEFINITION_SHAPE($,$,#342);
#16441=PRODUCT_DEFINITION_SHAPE($,$,#343);
#16442=PRODUCT_DEFINITION_SHAPE($,$,#344);
#16443=PRODUCT_DEFINITION_SHAPE($,$,#345);
#16444=PRODUCT_DEFINITION_SHAPE($,$,#346);
#16445=PRODUCT_DEFINITION_SHAPE($,$,#347);
#16446=PRODUCT_DEFINITION_SHAPE($,$,#348);
#16447=PRODUCT_DEFINITION_SHAPE($,$,#349);
#16448=PRODUCT_DEFINITION_SHAPE($,$,#350);
#16449=PRODUCT_DEFINITION_SHAPE($,$,#351);
#16450=PRODUCT_DEFINITION_SHAPE($,$,#352);
#16451=PRODUCT_DEFINITION_SHAPE($,$,#353);
#16452=PRODUCT_DEFINITION_SHAPE($,$,#354);
#16453=PRODUCT_DEFINITION_SHAPE($,$,#355);
#16454=PRODUCT_DEFINITION_SHAPE($,$,#356);
#16455=PRODUCT_DEFINITION_SHAPE($,$,#357);
#16456=PRODUCT_DEFINITION_SHAPE($,$,#358);
#16457=PRODUCT_DEFINITION_SHAPE($,$,#359);
#16458=PRODUCT_DEFINITION_SHAPE($,$,#360);
#16459=PRODUCT_DEFINITION_SHAPE($,$,#361);
#16460=PRODUCT_DEFINITION_SHAPE($,$,#362);
#16461=PRODUCT_DEFINITION_SHAPE($,$,#363);
#16462=PRODUCT_DEFINITION_SHAPE($,$,#364);
#16463=PRODUCT_DEFINITION_SHAPE($,$,#365);
#16464=PRODUCT_DEFINITION_SHAPE($,$,#366);
#16465=PRODUCT_DEFINITION_SHAPE($,$,#367);
#16466=PRODUCT_DEFINITION_SHAPE('',$,#16634);
#16467=PRODUCT_DEFINITION_SHAPE('',$,#16635);
#16468=PRODUCT_DEFINITION_SHAPE('',$,#16636);
#16469=PRODUCT_DEFINITION_SHAPE('',$,#16637);
#16470=PRODUCT_DEFINITION_SHAPE('',$,#16638);
#16471=PRODUCT_DEFINITION_SHAPE('',$,#16639);
#16472=PRODUCT_DEFINITION_SHAPE('',$,#16640);
#16473=PRODUCT_DEFINITION_SHAPE('',$,#16641);
#16474=PRODUCT_DEFINITION_SHAPE('',$,#16642);
#16475=PRODUCT_DEFINITION_SHAPE('',$,#16643);
#16476=PRODUCT_DEFINITION_SHAPE('',$,#16644);
#16477=PRODUCT_DEFINITION_SHAPE('',$,#16645);
#16478=PRODUCT_DEFINITION_SHAPE('',$,#16646);
#16479=PRODUCT_DEFINITION_SHAPE('',$,#16647);
#16480=PRODUCT_DEFINITION_SHAPE('',$,#16648);
#16481=PRODUCT_DEFINITION_SHAPE('',$,#16649);
#16482=PRODUCT_DEFINITION_SHAPE('',$,#16650);
#16483=PRODUCT_DEFINITION_SHAPE('',$,#16651);
#16484=PRODUCT_DEFINITION_SHAPE('',$,#16652);
#16485=PRODUCT_DEFINITION_SHAPE('',$,#16653);
#16486=PRODUCT_DEFINITION_SHAPE('',$,#16654);
#16487=PRODUCT_DEFINITION_SHAPE('',$,#16655);
#16488=PRODUCT_DEFINITION_SHAPE($,$,#368);
#16489=PRODUCT_DEFINITION_SHAPE($,$,#369);
#16490=PRODUCT_DEFINITION_SHAPE($,$,#370);
#16491=PRODUCT_DEFINITION_SHAPE($,$,#371);
#16492=PRODUCT_DEFINITION_SHAPE($,$,#372);
#16493=PRODUCT_DEFINITION_SHAPE($,$,#373);
#16494=PRODUCT_DEFINITION_SHAPE($,$,#374);
#16495=PRODUCT_DEFINITION_SHAPE($,$,#375);
#16496=PRODUCT_DEFINITION_SHAPE($,$,#376);
#16497=PRODUCT_DEFINITION_SHAPE($,$,#377);
#16498=PRODUCT_DEFINITION_SHAPE($,$,#378);
#16499=PRODUCT_DEFINITION_SHAPE($,$,#379);
#16500=PRODUCT_DEFINITION_SHAPE($,$,#380);
#16501=PRODUCT_DEFINITION_SHAPE($,$,#381);
#16502=PRODUCT_DEFINITION_SHAPE($,$,#382);
#16503=PRODUCT_DEFINITION_SHAPE($,$,#383);
#16504=PRODUCT_DEFINITION_SHAPE($,$,#384);
#16505=PRODUCT_DEFINITION_SHAPE($,$,#385);
#16506=PRODUCT_DEFINITION_SHAPE($,$,#386);
#16507=PRODUCT_DEFINITION_SHAPE($,$,#387);
#16508=PRODUCT_DEFINITION_SHAPE($,$,#388);
#16509=PRODUCT_DEFINITION_SHAPE($,$,#389);
#16510=PRODUCT_DEFINITION_SHAPE($,$,#390);
#16511=PRODUCT_DEFINITION_SHAPE($,$,#391);
#16512=PRODUCT_DEFINITION_SHAPE($,$,#392);
#16513=PRODUCT_DEFINITION_SHAPE($,$,#393);
#16514=PRODUCT_DEFINITION_SHAPE($,$,#394);
#16515=PRODUCT_DEFINITION_SHAPE($,$,#395);
#16516=PRODUCT_DEFINITION_SHAPE($,$,#396);
#16517=PRODUCT_DEFINITION_SHAPE($,$,#397);
#16518=PRODUCT_DEFINITION_SHAPE($,$,#398);
#16519=SHAPE_REPRESENTATION('',(#9040,#10190,#10191,#10192,#10193,#10194,
#10195,#10196,#10197,#10198,#10199),#16213);
#16520=SHAPE_REPRESENTATION('',(#9041,#9494,#9495,#9496,#9497,#9498,#9499,
#9500,#9501,#9502,#9503,#9504,#9505,#9506,#9507),#16214);
#16521=SHAPE_REPRESENTATION('',(#9042),#16215);
#16522=SHAPE_REPRESENTATION('',(#9109),#16216);
#16523=SHAPE_REPRESENTATION('',(#9181),#16217);
#16524=SHAPE_REPRESENTATION('',(#9206),#16218);
#16525=SHAPE_REPRESENTATION('',(#9230,#9369,#9370,#9371,#9372,#9373),#16219);
#16526=SHAPE_REPRESENTATION('',(#9231),#16220);
#16527=SHAPE_REPRESENTATION('',(#9251),#16221);
#16528=SHAPE_REPRESENTATION('',(#9271),#16222);
#16529=SHAPE_REPRESENTATION('',(#9290),#16223);
#16530=SHAPE_REPRESENTATION('',(#9352),#16224);
#16531=SHAPE_REPRESENTATION('',(#9374),#16225);
#16532=SHAPE_REPRESENTATION('',(#9381),#16226);
#16533=SHAPE_REPRESENTATION('',(#9388,#9525,#9526,#9527,#9528,#9529,#9530,
#9531),#16227);
#16534=SHAPE_REPRESENTATION('',(#9389),#16228);
#16535=SHAPE_REPRESENTATION('',(#9411),#16229);
#16536=SHAPE_REPRESENTATION('',(#9453),#16230);
#16537=SHAPE_REPRESENTATION('',(#9468),#16231);
#16538=SHAPE_REPRESENTATION('',(#9508),#16232);
#16539=SHAPE_REPRESENTATION('',(#9532,#9888,#9889,#9890,#9891,#9892,#9893,
#9894,#9895,#9896,#9897),#16233);
#16540=SHAPE_REPRESENTATION('',(#9533),#16234);
#16541=SHAPE_REPRESENTATION('',(#9568),#16235);
#16542=SHAPE_REPRESENTATION('',(#9582),#16236);
#16543=SHAPE_REPRESENTATION('',(#9591),#16237);
#16544=SHAPE_REPRESENTATION('',(#9600),#16238);
#16545=SHAPE_REPRESENTATION('',(#9609,#9898,#9899,#9900,#9901,#9902,#9903,
#9904,#9905,#9906,#9907),#16239);
#16546=SHAPE_REPRESENTATION('',(#9610),#16240);
#16547=SHAPE_REPRESENTATION('',(#9645),#16241);
#16548=SHAPE_REPRESENTATION('',(#9659),#16242);
#16549=SHAPE_REPRESENTATION('',(#9668),#16243);
#16550=SHAPE_REPRESENTATION('',(#9677),#16244);
#16551=SHAPE_REPRESENTATION('',(#9686,#9908,#9909,#9910,#9911,#9912,#9913,
#9914,#9915,#9916,#9917),#16245);
#16552=SHAPE_REPRESENTATION('',(#9687),#16246);
#16553=SHAPE_REPRESENTATION('',(#9722),#16247);
#16554=SHAPE_REPRESENTATION('',(#9736),#16248);
#16555=SHAPE_REPRESENTATION('',(#9745),#16249);
#16556=SHAPE_REPRESENTATION('',(#9754),#16250);
#16557=SHAPE_REPRESENTATION('',(#9763,#9918,#9919,#9920,#9921,#9922,#9923,
#9924,#9925,#9926,#9927),#16251);
#16558=SHAPE_REPRESENTATION('',(#9764),#16252);
#16559=SHAPE_REPRESENTATION('',(#9799),#16253);
#16560=SHAPE_REPRESENTATION('',(#9813),#16254);
#16561=SHAPE_REPRESENTATION('',(#9822),#16255);
#16562=SHAPE_REPRESENTATION('',(#9831),#16256);
#16563=SHAPE_REPRESENTATION('',(#9840),#16257);
#16564=SHAPE_REPRESENTATION('',(#9864),#16258);
#16565=SHAPE_REPRESENTATION('',(#9928,#10174,#10175,#10176,#10177),#16259);
#16566=SHAPE_REPRESENTATION('',(#9929),#16260);
#16567=SHAPE_REPRESENTATION('',(#9938),#16261);
#16568=SHAPE_REPRESENTATION('',(#9947),#16262);
#16569=SHAPE_REPRESENTATION('',(#9956,#10178,#10179,#10180,#10181),#16263);
#16570=SHAPE_REPRESENTATION('',(#9957),#16264);
#16571=SHAPE_REPRESENTATION('',(#9966),#16265);
#16572=SHAPE_REPRESENTATION('',(#9975),#16266);
#16573=SHAPE_REPRESENTATION('',(#9984,#10182,#10183,#10184,#10185),#16267);
#16574=SHAPE_REPRESENTATION('',(#9985),#16268);
#16575=SHAPE_REPRESENTATION('',(#9994),#16269);
#16576=SHAPE_REPRESENTATION('',(#10003),#16270);
#16577=SHAPE_REPRESENTATION('',(#10012,#10186,#10187,#10188,#10189),#16271);
#16578=SHAPE_REPRESENTATION('',(#10013),#16272);
#16579=SHAPE_REPRESENTATION('',(#10022),#16273);
#16580=SHAPE_REPRESENTATION('',(#10031),#16274);
#16581=SHAPE_REPRESENTATION('',(#10040,#10169,#10170,#10171,#10172,#10173),
#16275);
#16582=SHAPE_REPRESENTATION('',(#10041),#16276);
#16583=SHAPE_REPRESENTATION('',(#10061),#16277);
#16584=SHAPE_REPRESENTATION('',(#10081),#16278);
#16585=SHAPE_REPRESENTATION('',(#10098),#16279);
#16586=SHAPE_REPRESENTATION('',(#10152),#16280);
#16587=PRODUCT_DEFINITION_CONTEXT('part definition',#16793,'design');
#16588=PRODUCT_DEFINITION('PAT-107','PAT-107',#16656,
#16587);
#16589=PRODUCT_DEFINITION('Base and centre bearing',
'Base and centre bearing',#16657,#16587);
#16590=PRODUCT_DEFINITION('Base','Base',#16658,#16587);
#16591=PRODUCT_DEFINITION('Centre housing','Centre housing',#16659,#16587);
#16592=PRODUCT_DEFINITION('Bearing cap','Bearing cap',#16660,#16587);
#16593=PRODUCT_DEFINITION('M6x18 mounting screw','M6x18 mounting screw',
#16661,#16587);
#16594=PRODUCT_DEFINITION('Sealed Ball Bearing - 25 x 52 x 15 mm',
'Sealed Ball Bearing - 25 x 52 x 15 mm',#16662,#16587);
#16595=PRODUCT_DEFINITION('Inner ring','Inner ring',#16663,#16587);
#16596=PRODUCT_DEFINITION('Outer ring','Outer ring',#16664,#16587);
#16597=PRODUCT_DEFINITION('Balls','Balls',#16665,#16587);
#16598=PRODUCT_DEFINITION('Cage','Cage',#16666,#16587);
#16599=PRODUCT_DEFINITION('Seals 2RS','Seals 2RS',#16667,#16587);
#16600=PRODUCT_DEFINITION('Bonded foot','Bonded foot',#16668,#16587);
#16601=PRODUCT_DEFINITION('Bonded foot (1)','Bonded foot (1)',#16669,#16587);
#16602=PRODUCT_DEFINITION('Turntable','Turntable',#16670,#16587);
#16603=PRODUCT_DEFINITION('Centre spindle','Centre spindle',#16671,#16587);
#16604=PRODUCT_DEFINITION('Table disc','Table disc',#16672,#16587);
#16605=PRODUCT_DEFINITION('Retention collar','Retention collar',#16673,
#16587);
#16606=PRODUCT_DEFINITION('Cap Screw - M4x16','Cap Screw - M4x16',#16674,
#16587);
#16607=PRODUCT_DEFINITION('Socket Set Screw - M5x8',
'Socket Set Screw - M5x8',#16675,#16587);
#16608=PRODUCT_DEFINITION('Mount 1','Mount 1',#16676,#16587);
#16609=PRODUCT_DEFINITION('Roller bracket','Roller bracket',#16677,#16587);
#16610=PRODUCT_DEFINITION('Roller axle','Roller axle',#16678,#16587);
#16611=PRODUCT_DEFINITION('Inner race spacer','Inner race spacer',#16679,
#16587);
#16612=PRODUCT_DEFINITION('Inner race spacer (1)','Inner race spacer (1)',
#16680,#16587);
#16613=PRODUCT_DEFINITION('Axle keeper','Axle keeper',#16681,#16587);
#16614=PRODUCT_DEFINITION('Mount 2','Mount 2',#16682,#16587);
#16615=PRODUCT_DEFINITION('Roller bracket (1)','Roller bracket (1)',#16683,
#16587);
#16616=PRODUCT_DEFINITION('Roller axle (1)','Roller axle (1)',#16684,#16587);
#16617=PRODUCT_DEFINITION('Inner race spacer (2)','Inner race spacer (2)',
#16685,#16587);
#16618=PRODUCT_DEFINITION('Inner race spacer (3)','Inner race spacer (3)',
#16686,#16587);
#16619=PRODUCT_DEFINITION('Axle keeper (1)','Axle keeper (1)',#16687,#16587);
#16620=PRODUCT_DEFINITION('Mount 3','Mount 3',#16688,#16587);
#16621=PRODUCT_DEFINITION('Roller bracket (2)','Roller bracket (2)',#16689,
#16587);
#16622=PRODUCT_DEFINITION('Roller axle (2)','Roller axle (2)',#16690,#16587);
#16623=PRODUCT_DEFINITION('Inner race spacer (4)','Inner race spacer (4)',
#16691,#16587);
#16624=PRODUCT_DEFINITION('Inner race spacer (5)','Inner race spacer (5)',
#16692,#16587);
#16625=PRODUCT_DEFINITION('Axle keeper (2)','Axle keeper (2)',#16693,#16587);
#16626=PRODUCT_DEFINITION('Mount 4','Mount 4',#16694,#16587);
#16627=PRODUCT_DEFINITION('Roller bracket (3)','Roller bracket (3)',#16695,
#16587);
#16628=PRODUCT_DEFINITION('Roller axle (3)','Roller axle (3)',#16696,#16587);
#16629=PRODUCT_DEFINITION('Inner race spacer (6)','Inner race spacer (6)',
#16697,#16587);
#16630=PRODUCT_DEFINITION('Inner race spacer (7)','Inner race spacer (7)',
#16698,#16587);
#16631=PRODUCT_DEFINITION('Axle keeper (3)','Axle keeper (3)',#16699,#16587);
#16632=PRODUCT_DEFINITION('M5x14 Cap Screw','M5x14 Cap Screw',#16700,#16587);
#16633=PRODUCT_DEFINITION('M4x10 Cap Screw','M4x10 Cap Screw',#16701,#16587);
#16634=PRODUCT_DEFINITION('Roller 1','Roller 1',#16702,#16587);
#16635=PRODUCT_DEFINITION('Roller tread','Roller tread',#16703,#16587);
#16636=PRODUCT_DEFINITION('Outer race retainer','Outer race retainer',#16704,
#16587);
#16637=PRODUCT_DEFINITION('Outer race retainer (1)',
'Outer race retainer (1)',#16705,#16587);
#16638=PRODUCT_DEFINITION('Roller 2','Roller 2',#16706,#16587);
#16639=PRODUCT_DEFINITION('Roller tread (1)','Roller tread (1)',#16707,#16587);
#16640=PRODUCT_DEFINITION('Outer race retainer (2)',
'Outer race retainer (2)',#16708,#16587);
#16641=PRODUCT_DEFINITION('Outer race retainer (3)',
'Outer race retainer (3)',#16709,#16587);
#16642=PRODUCT_DEFINITION('Roller 3','Roller 3',#16710,#16587);
#16643=PRODUCT_DEFINITION('Roller tread (2)','Roller tread (2)',#16711,#16587);
#16644=PRODUCT_DEFINITION('Outer race retainer (4)',
'Outer race retainer (4)',#16712,#16587);
#16645=PRODUCT_DEFINITION('Outer race retainer (5)',
'Outer race retainer (5)',#16713,#16587);
#16646=PRODUCT_DEFINITION('Roller 4','Roller 4',#16714,#16587);
#16647=PRODUCT_DEFINITION('Roller tread (3)','Roller tread (3)',#16715,#16587);
#16648=PRODUCT_DEFINITION('Outer race retainer (6)',
'Outer race retainer (6)',#16716,#16587);
#16649=PRODUCT_DEFINITION('Outer race retainer (7)',
'Outer race retainer (7)',#16717,#16587);
#16650=PRODUCT_DEFINITION('Sealed Ball Bearing - 10 x 30 x 9 mm',
'Sealed Ball Bearing - 10 x 30 x 9 mm',#16718,#16587);
#16651=PRODUCT_DEFINITION('Inner ring (1)','Inner ring (1)',#16719,#16587);
#16652=PRODUCT_DEFINITION('Outer ring (1)','Outer ring (1)',#16720,#16587);
#16653=PRODUCT_DEFINITION('Balls (1)','Balls (1)',#16721,#16587);
#16654=PRODUCT_DEFINITION('Cage (1)','Cage (1)',#16722,#16587);
#16655=PRODUCT_DEFINITION('Seals 2RS (1)','Seals 2RS (1)',#16723,#16587);
#16656=PRODUCT_DEFINITION_FORMATION('',$,#16795);
#16657=PRODUCT_DEFINITION_FORMATION('',$,#16796);
#16658=PRODUCT_DEFINITION_FORMATION('',$,#16797);
#16659=PRODUCT_DEFINITION_FORMATION('',$,#16798);
#16660=PRODUCT_DEFINITION_FORMATION('',$,#16799);
#16661=PRODUCT_DEFINITION_FORMATION('',$,#16800);
#16662=PRODUCT_DEFINITION_FORMATION('',$,#16801);
#16663=PRODUCT_DEFINITION_FORMATION('',$,#16802);
#16664=PRODUCT_DEFINITION_FORMATION('',$,#16803);
#16665=PRODUCT_DEFINITION_FORMATION('',$,#16804);
#16666=PRODUCT_DEFINITION_FORMATION('',$,#16805);
#16667=PRODUCT_DEFINITION_FORMATION('',$,#16806);
#16668=PRODUCT_DEFINITION_FORMATION('',$,#16807);
#16669=PRODUCT_DEFINITION_FORMATION('',$,#16808);
#16670=PRODUCT_DEFINITION_FORMATION('',$,#16809);
#16671=PRODUCT_DEFINITION_FORMATION('',$,#16810);
#16672=PRODUCT_DEFINITION_FORMATION('',$,#16811);
#16673=PRODUCT_DEFINITION_FORMATION('',$,#16812);
#16674=PRODUCT_DEFINITION_FORMATION('',$,#16813);
#16675=PRODUCT_DEFINITION_FORMATION('',$,#16814);
#16676=PRODUCT_DEFINITION_FORMATION('',$,#16815);
#16677=PRODUCT_DEFINITION_FORMATION('',$,#16816);
#16678=PRODUCT_DEFINITION_FORMATION('',$,#16817);
#16679=PRODUCT_DEFINITION_FORMATION('',$,#16818);
#16680=PRODUCT_DEFINITION_FORMATION('',$,#16819);
#16681=PRODUCT_DEFINITION_FORMATION('',$,#16820);
#16682=PRODUCT_DEFINITION_FORMATION('',$,#16821);
#16683=PRODUCT_DEFINITION_FORMATION('',$,#16822);
#16684=PRODUCT_DEFINITION_FORMATION('',$,#16823);
#16685=PRODUCT_DEFINITION_FORMATION('',$,#16824);
#16686=PRODUCT_DEFINITION_FORMATION('',$,#16825);
#16687=PRODUCT_DEFINITION_FORMATION('',$,#16826);
#16688=PRODUCT_DEFINITION_FORMATION('',$,#16827);
#16689=PRODUCT_DEFINITION_FORMATION('',$,#16828);
#16690=PRODUCT_DEFINITION_FORMATION('',$,#16829);
#16691=PRODUCT_DEFINITION_FORMATION('',$,#16830);
#16692=PRODUCT_DEFINITION_FORMATION('',$,#16831);
#16693=PRODUCT_DEFINITION_FORMATION('',$,#16832);
#16694=PRODUCT_DEFINITION_FORMATION('',$,#16833);
#16695=PRODUCT_DEFINITION_FORMATION('',$,#16834);
#16696=PRODUCT_DEFINITION_FORMATION('',$,#16835);
#16697=PRODUCT_DEFINITION_FORMATION('',$,#16836);
#16698=PRODUCT_DEFINITION_FORMATION('',$,#16837);
#16699=PRODUCT_DEFINITION_FORMATION('',$,#16838);
#16700=PRODUCT_DEFINITION_FORMATION('',$,#16839);
#16701=PRODUCT_DEFINITION_FORMATION('',$,#16840);
#16702=PRODUCT_DEFINITION_FORMATION('',$,#16841);
#16703=PRODUCT_DEFINITION_FORMATION('',$,#16842);
#16704=PRODUCT_DEFINITION_FORMATION('',$,#16843);
#16705=PRODUCT_DEFINITION_FORMATION('',$,#16844);
#16706=PRODUCT_DEFINITION_FORMATION('',$,#16845);
#16707=PRODUCT_DEFINITION_FORMATION('',$,#16846);
#16708=PRODUCT_DEFINITION_FORMATION('',$,#16847);
#16709=PRODUCT_DEFINITION_FORMATION('',$,#16848);
#16710=PRODUCT_DEFINITION_FORMATION('',$,#16849);
#16711=PRODUCT_DEFINITION_FORMATION('',$,#16850);
#16712=PRODUCT_DEFINITION_FORMATION('',$,#16851);
#16713=PRODUCT_DEFINITION_FORMATION('',$,#16852);
#16714=PRODUCT_DEFINITION_FORMATION('',$,#16853);
#16715=PRODUCT_DEFINITION_FORMATION('',$,#16854);
#16716=PRODUCT_DEFINITION_FORMATION('',$,#16855);
#16717=PRODUCT_DEFINITION_FORMATION('',$,#16856);
#16718=PRODUCT_DEFINITION_FORMATION('',$,#16857);
#16719=PRODUCT_DEFINITION_FORMATION('',$,#16858);
#16720=PRODUCT_DEFINITION_FORMATION('',$,#16859);
#16721=PRODUCT_DEFINITION_FORMATION('',$,#16860);
#16722=PRODUCT_DEFINITION_FORMATION('',$,#16861);
#16723=PRODUCT_DEFINITION_FORMATION('',$,#16862);
#16724=PRODUCT_RELATED_PRODUCT_CATEGORY('PAT-107','PAT-107',(#16795));
#16725=PRODUCT_RELATED_PRODUCT_CATEGORY('Base and centre bearing',
'Base and centre bearing',(#16796));
#16726=PRODUCT_RELATED_PRODUCT_CATEGORY('Base','Base',(#16797));
#16727=PRODUCT_RELATED_PRODUCT_CATEGORY('Centre housing',
'Centre housing',(#16798));
#16728=PRODUCT_RELATED_PRODUCT_CATEGORY('Bearing cap','Bearing cap',(#16799));
#16729=PRODUCT_RELATED_PRODUCT_CATEGORY('M6x18 mounting screw',
'M6x18 mounting screw',(#16800));
#16730=PRODUCT_RELATED_PRODUCT_CATEGORY(
'Sealed Ball Bearing - 25 x 52 x 15 mm',
'Sealed Ball Bearing - 25 x 52 x 15 mm',(#16801));
#16731=PRODUCT_RELATED_PRODUCT_CATEGORY('Inner ring','Inner ring',(#16802));
#16732=PRODUCT_RELATED_PRODUCT_CATEGORY('Outer ring','Outer ring',(#16803));
#16733=PRODUCT_RELATED_PRODUCT_CATEGORY('Balls','Balls',(#16804));
#16734=PRODUCT_RELATED_PRODUCT_CATEGORY('Cage','Cage',(#16805));
#16735=PRODUCT_RELATED_PRODUCT_CATEGORY('Seals 2RS','Seals 2RS',(#16806));
#16736=PRODUCT_RELATED_PRODUCT_CATEGORY('Bonded foot','Bonded foot',(#16807));
#16737=PRODUCT_RELATED_PRODUCT_CATEGORY('Bonded foot (1)',
'Bonded foot (1)',(#16808));
#16738=PRODUCT_RELATED_PRODUCT_CATEGORY('Turntable','Turntable',(#16809));
#16739=PRODUCT_RELATED_PRODUCT_CATEGORY('Centre spindle',
'Centre spindle',(#16810));
#16740=PRODUCT_RELATED_PRODUCT_CATEGORY('Table disc','Table disc',(#16811));
#16741=PRODUCT_RELATED_PRODUCT_CATEGORY('Retention collar',
'Retention collar',(#16812));
#16742=PRODUCT_RELATED_PRODUCT_CATEGORY('Cap Screw - M4x16',
'Cap Screw - M4x16',(#16813));
#16743=PRODUCT_RELATED_PRODUCT_CATEGORY('Socket Set Screw - M5x8',
'Socket Set Screw - M5x8',(#16814));
#16744=PRODUCT_RELATED_PRODUCT_CATEGORY('Mount 1','Mount 1',(#16815));
#16745=PRODUCT_RELATED_PRODUCT_CATEGORY('Roller bracket',
'Roller bracket',(#16816));
#16746=PRODUCT_RELATED_PRODUCT_CATEGORY('Roller axle','Roller axle',(#16817));
#16747=PRODUCT_RELATED_PRODUCT_CATEGORY('Inner race spacer',
'Inner race spacer',(#16818));
#16748=PRODUCT_RELATED_PRODUCT_CATEGORY('Inner race spacer (1)',
'Inner race spacer (1)',(#16819));
#16749=PRODUCT_RELATED_PRODUCT_CATEGORY('Axle keeper','Axle keeper',(#16820));
#16750=PRODUCT_RELATED_PRODUCT_CATEGORY('Mount 2','Mount 2',(#16821));
#16751=PRODUCT_RELATED_PRODUCT_CATEGORY('Roller bracket (1)',
'Roller bracket (1)',(#16822));
#16752=PRODUCT_RELATED_PRODUCT_CATEGORY('Roller axle (1)',
'Roller axle (1)',(#16823));
#16753=PRODUCT_RELATED_PRODUCT_CATEGORY('Inner race spacer (2)',
'Inner race spacer (2)',(#16824));
#16754=PRODUCT_RELATED_PRODUCT_CATEGORY('Inner race spacer (3)',
'Inner race spacer (3)',(#16825));
#16755=PRODUCT_RELATED_PRODUCT_CATEGORY('Axle keeper (1)',
'Axle keeper (1)',(#16826));
#16756=PRODUCT_RELATED_PRODUCT_CATEGORY('Mount 3','Mount 3',(#16827));
#16757=PRODUCT_RELATED_PRODUCT_CATEGORY('Roller bracket (2)',
'Roller bracket (2)',(#16828));
#16758=PRODUCT_RELATED_PRODUCT_CATEGORY('Roller axle (2)',
'Roller axle (2)',(#16829));
#16759=PRODUCT_RELATED_PRODUCT_CATEGORY('Inner race spacer (4)',
'Inner race spacer (4)',(#16830));
#16760=PRODUCT_RELATED_PRODUCT_CATEGORY('Inner race spacer (5)',
'Inner race spacer (5)',(#16831));
#16761=PRODUCT_RELATED_PRODUCT_CATEGORY('Axle keeper (2)',
'Axle keeper (2)',(#16832));
#16762=PRODUCT_RELATED_PRODUCT_CATEGORY('Mount 4','Mount 4',(#16833));
#16763=PRODUCT_RELATED_PRODUCT_CATEGORY('Roller bracket (3)',
'Roller bracket (3)',(#16834));
#16764=PRODUCT_RELATED_PRODUCT_CATEGORY('Roller axle (3)',
'Roller axle (3)',(#16835));
#16765=PRODUCT_RELATED_PRODUCT_CATEGORY('Inner race spacer (6)',
'Inner race spacer (6)',(#16836));
#16766=PRODUCT_RELATED_PRODUCT_CATEGORY('Inner race spacer (7)',
'Inner race spacer (7)',(#16837));
#16767=PRODUCT_RELATED_PRODUCT_CATEGORY('Axle keeper (3)',
'Axle keeper (3)',(#16838));
#16768=PRODUCT_RELATED_PRODUCT_CATEGORY('M5x14 Cap Screw',
'M5x14 Cap Screw',(#16839));
#16769=PRODUCT_RELATED_PRODUCT_CATEGORY('M4x10 Cap Screw',
'M4x10 Cap Screw',(#16840));
#16770=PRODUCT_RELATED_PRODUCT_CATEGORY('Roller 1','Roller 1',(#16841));
#16771=PRODUCT_RELATED_PRODUCT_CATEGORY('Roller tread','Roller tread',(#16842));
#16772=PRODUCT_RELATED_PRODUCT_CATEGORY('Outer race retainer',
'Outer race retainer',(#16843));
#16773=PRODUCT_RELATED_PRODUCT_CATEGORY('Outer race retainer (1)',
'Outer race retainer (1)',(#16844));
#16774=PRODUCT_RELATED_PRODUCT_CATEGORY('Roller 2','Roller 2',(#16845));
#16775=PRODUCT_RELATED_PRODUCT_CATEGORY('Roller tread (1)',
'Roller tread (1)',(#16846));
#16776=PRODUCT_RELATED_PRODUCT_CATEGORY('Outer race retainer (2)',
'Outer race retainer (2)',(#16847));
#16777=PRODUCT_RELATED_PRODUCT_CATEGORY('Outer race retainer (3)',
'Outer race retainer (3)',(#16848));
#16778=PRODUCT_RELATED_PRODUCT_CATEGORY('Roller 3','Roller 3',(#16849));
#16779=PRODUCT_RELATED_PRODUCT_CATEGORY('Roller tread (2)',
'Roller tread (2)',(#16850));
#16780=PRODUCT_RELATED_PRODUCT_CATEGORY('Outer race retainer (4)',
'Outer race retainer (4)',(#16851));
#16781=PRODUCT_RELATED_PRODUCT_CATEGORY('Outer race retainer (5)',
'Outer race retainer (5)',(#16852));
#16782=PRODUCT_RELATED_PRODUCT_CATEGORY('Roller 4','Roller 4',(#16853));
#16783=PRODUCT_RELATED_PRODUCT_CATEGORY('Roller tread (3)',
'Roller tread (3)',(#16854));
#16784=PRODUCT_RELATED_PRODUCT_CATEGORY('Outer race retainer (6)',
'Outer race retainer (6)',(#16855));
#16785=PRODUCT_RELATED_PRODUCT_CATEGORY('Outer race retainer (7)',
'Outer race retainer (7)',(#16856));
#16786=PRODUCT_RELATED_PRODUCT_CATEGORY(
'Sealed Ball Bearing - 10 x 30 x 9 mm',
'Sealed Ball Bearing - 10 x 30 x 9 mm',(#16857));
#16787=PRODUCT_RELATED_PRODUCT_CATEGORY('Inner ring (1)',
'Inner ring (1)',(#16858));
#16788=PRODUCT_RELATED_PRODUCT_CATEGORY('Outer ring (1)',
'Outer ring (1)',(#16859));
#16789=PRODUCT_RELATED_PRODUCT_CATEGORY('Balls (1)','Balls (1)',(#16860));
#16790=PRODUCT_RELATED_PRODUCT_CATEGORY('Cage (1)','Cage (1)',(#16861));
#16791=PRODUCT_RELATED_PRODUCT_CATEGORY('Seals 2RS (1)','Seals 2RS (1)',
(#16862));
#16792=APPLICATION_PROTOCOL_DEFINITION('international standard',
'automotive_design',2009,#16793);
#16793=APPLICATION_CONTEXT(
'Core Data for Automotive Mechanical Design Process');
#16794=PRODUCT_CONTEXT('part definition',#16793,'mechanical');
#16795=PRODUCT('PAT-107','PAT-107',
'PAT-107',(#16794));
#16796=PRODUCT('Base and centre bearing','Base and centre bearing',
'Base and centre bearing',(#16794));
#16797=PRODUCT('Base','Base','Base',(#16794));
#16798=PRODUCT('Centre housing','Centre housing','Centre housing',(#16794));
#16799=PRODUCT('Bearing cap','Bearing cap','Bearing cap',(#16794));
#16800=PRODUCT('M6x18 mounting screw','M6x18 mounting screw',
'M6x18 mounting screw',(#16794));
#16801=PRODUCT('Sealed Ball Bearing - 25 x 52 x 15 mm',
'Sealed Ball Bearing - 25 x 52 x 15 mm',
'Sealed Ball Bearing - 25 x 52 x 15 mm',(#16794));
#16802=PRODUCT('Inner ring','Inner ring','Inner ring',(#16794));
#16803=PRODUCT('Outer ring','Outer ring','Outer ring',(#16794));
#16804=PRODUCT('Balls','Balls','Balls',(#16794));
#16805=PRODUCT('Cage','Cage','Cage',(#16794));
#16806=PRODUCT('Seals 2RS','Seals 2RS','Seals 2RS',(#16794));
#16807=PRODUCT('Bonded foot','Bonded foot','Bonded foot',(#16794));
#16808=PRODUCT('Bonded foot (1)','Bonded foot (1)','Bonded foot (1)',(#16794));
#16809=PRODUCT('Turntable','Turntable','Turntable',(#16794));
#16810=PRODUCT('Centre spindle','Centre spindle','Centre spindle',(#16794));
#16811=PRODUCT('Table disc','Table disc','Table disc',(#16794));
#16812=PRODUCT('Retention collar','Retention collar','Retention collar',
(#16794));
#16813=PRODUCT('Cap Screw - M4x16','Cap Screw - M4x16',
'Cap Screw - M4x16',(#16794));
#16814=PRODUCT('Socket Set Screw - M5x8','Socket Set Screw - M5x8',
'Socket Set Screw - M5x8',(#16794));
#16815=PRODUCT('Mount 1','Mount 1','Mount 1',(#16794));
#16816=PRODUCT('Roller bracket','Roller bracket','Roller bracket',(#16794));
#16817=PRODUCT('Roller axle','Roller axle','Roller axle',(#16794));
#16818=PRODUCT('Inner race spacer','Inner race spacer',
'Inner race spacer',(#16794));
#16819=PRODUCT('Inner race spacer (1)','Inner race spacer (1)',
'Inner race spacer (1)',(#16794));
#16820=PRODUCT('Axle keeper','Axle keeper','Axle keeper',(#16794));
#16821=PRODUCT('Mount 2','Mount 2','Mount 2',(#16794));
#16822=PRODUCT('Roller bracket (1)','Roller bracket (1)','Roller bracket (1)',
(#16794));
#16823=PRODUCT('Roller axle (1)','Roller axle (1)','Roller axle (1)',(#16794));
#16824=PRODUCT('Inner race spacer (2)','Inner race spacer (2)',
'Inner race spacer (2)',(#16794));
#16825=PRODUCT('Inner race spacer (3)','Inner race spacer (3)',
'Inner race spacer (3)',(#16794));
#16826=PRODUCT('Axle keeper (1)','Axle keeper (1)','Axle keeper (1)',(#16794));
#16827=PRODUCT('Mount 3','Mount 3','Mount 3',(#16794));
#16828=PRODUCT('Roller bracket (2)','Roller bracket (2)','Roller bracket (2)',
(#16794));
#16829=PRODUCT('Roller axle (2)','Roller axle (2)','Roller axle (2)',(#16794));
#16830=PRODUCT('Inner race spacer (4)','Inner race spacer (4)',
'Inner race spacer (4)',(#16794));
#16831=PRODUCT('Inner race spacer (5)','Inner race spacer (5)',
'Inner race spacer (5)',(#16794));
#16832=PRODUCT('Axle keeper (2)','Axle keeper (2)','Axle keeper (2)',(#16794));
#16833=PRODUCT('Mount 4','Mount 4','Mount 4',(#16794));
#16834=PRODUCT('Roller bracket (3)','Roller bracket (3)','Roller bracket (3)',
(#16794));
#16835=PRODUCT('Roller axle (3)','Roller axle (3)','Roller axle (3)',(#16794));
#16836=PRODUCT('Inner race spacer (6)','Inner race spacer (6)',
'Inner race spacer (6)',(#16794));
#16837=PRODUCT('Inner race spacer (7)','Inner race spacer (7)',
'Inner race spacer (7)',(#16794));
#16838=PRODUCT('Axle keeper (3)','Axle keeper (3)','Axle keeper (3)',(#16794));
#16839=PRODUCT('M5x14 Cap Screw','M5x14 Cap Screw','M5x14 Cap Screw',(#16794));
#16840=PRODUCT('M4x10 Cap Screw','M4x10 Cap Screw','M4x10 Cap Screw',(#16794));
#16841=PRODUCT('Roller 1','Roller 1','Roller 1',(#16794));
#16842=PRODUCT('Roller tread','Roller tread','Roller tread',(#16794));
#16843=PRODUCT('Outer race retainer','Outer race retainer',
'Outer race retainer',(#16794));
#16844=PRODUCT('Outer race retainer (1)','Outer race retainer (1)',
'Outer race retainer (1)',(#16794));
#16845=PRODUCT('Roller 2','Roller 2','Roller 2',(#16794));
#16846=PRODUCT('Roller tread (1)','Roller tread (1)','Roller tread (1)',(#16794));
#16847=PRODUCT('Outer race retainer (2)','Outer race retainer (2)',
'Outer race retainer (2)',(#16794));
#16848=PRODUCT('Outer race retainer (3)','Outer race retainer (3)',
'Outer race retainer (3)',(#16794));
#16849=PRODUCT('Roller 3','Roller 3','Roller 3',(#16794));
#16850=PRODUCT('Roller tread (2)','Roller tread (2)','Roller tread (2)',(#16794));
#16851=PRODUCT('Outer race retainer (4)','Outer race retainer (4)',
'Outer race retainer (4)',(#16794));
#16852=PRODUCT('Outer race retainer (5)','Outer race retainer (5)',
'Outer race retainer (5)',(#16794));
#16853=PRODUCT('Roller 4','Roller 4','Roller 4',(#16794));
#16854=PRODUCT('Roller tread (3)','Roller tread (3)','Roller tread (3)',(#16794));
#16855=PRODUCT('Outer race retainer (6)','Outer race retainer (6)',
'Outer race retainer (6)',(#16794));
#16856=PRODUCT('Outer race retainer (7)','Outer race retainer (7)',
'Outer race retainer (7)',(#16794));
#16857=PRODUCT('Sealed Ball Bearing - 10 x 30 x 9 mm',
'Sealed Ball Bearing - 10 x 30 x 9 mm',
'Sealed Ball Bearing - 10 x 30 x 9 mm',(#16794));
#16858=PRODUCT('Inner ring (1)','Inner ring (1)','Inner ring (1)',(#16794));
#16859=PRODUCT('Outer ring (1)','Outer ring (1)','Outer ring (1)',(#16794));
#16860=PRODUCT('Balls (1)','Balls (1)','Balls (1)',(#16794));
#16861=PRODUCT('Cage (1)','Cage (1)','Cage (1)',(#16794));
#16862=PRODUCT('Seals 2RS (1)','Seals 2RS (1)','Seals 2RS (1)',(#16794));
#16863=PRESENTATION_STYLE_ASSIGNMENT((#16869));
#16864=PRESENTATION_STYLE_ASSIGNMENT((#16870));
#16865=PRESENTATION_STYLE_ASSIGNMENT((#16871));
#16866=PRESENTATION_STYLE_ASSIGNMENT((#16872));
#16867=PRESENTATION_STYLE_ASSIGNMENT((#16873));
#16868=PRESENTATION_STYLE_ASSIGNMENT((#16874));
#16869=SURFACE_STYLE_USAGE(.BOTH.,#16875);
#16870=SURFACE_STYLE_USAGE(.BOTH.,#16876);
#16871=SURFACE_STYLE_USAGE(.BOTH.,#16877);
#16872=SURFACE_STYLE_USAGE(.BOTH.,#16878);
#16873=SURFACE_STYLE_USAGE(.BOTH.,#16879);
#16874=SURFACE_STYLE_USAGE(.BOTH.,#16880);
#16875=SURFACE_SIDE_STYLE('',(#16881));
#16876=SURFACE_SIDE_STYLE('',(#16882));
#16877=SURFACE_SIDE_STYLE('',(#16883));
#16878=SURFACE_SIDE_STYLE('',(#16884));
#16879=SURFACE_SIDE_STYLE('',(#16885));
#16880=SURFACE_SIDE_STYLE('',(#16886));
#16881=SURFACE_STYLE_FILL_AREA(#16887);
#16882=SURFACE_STYLE_FILL_AREA(#16888);
#16883=SURFACE_STYLE_FILL_AREA(#16889);
#16884=SURFACE_STYLE_FILL_AREA(#16890);
#16885=SURFACE_STYLE_FILL_AREA(#16891);
#16886=SURFACE_STYLE_FILL_AREA(#16892);
#16887=FILL_AREA_STYLE('Steel - Satin',(#16893));
#16888=FILL_AREA_STYLE('CAD Library Painted - Deep blue',(#16894));
#16889=FILL_AREA_STYLE('CAD Library Painted - Engineering blue',(#16895));
#16890=FILL_AREA_STYLE('CAD Library Painted - Steel gray',(#16896));
#16891=FILL_AREA_STYLE('CAD Library Painted - Graphite',(#16897));
#16892=FILL_AREA_STYLE('CAD Library Painted - Light blue',(#16898));
#16893=FILL_AREA_STYLE_COLOUR('Steel - Satin',#16899);
#16894=FILL_AREA_STYLE_COLOUR('CAD Library Painted - Deep blue',#16900);
#16895=FILL_AREA_STYLE_COLOUR('CAD Library Painted - Engineering blue',
#16901);
#16896=FILL_AREA_STYLE_COLOUR('CAD Library Painted - Steel gray',#16902);
#16897=FILL_AREA_STYLE_COLOUR('CAD Library Painted - Graphite',#16903);
#16898=FILL_AREA_STYLE_COLOUR('CAD Library Painted - Light blue',#16904);
#16899=COLOUR_RGB('Steel - Satin',0.627450980392157,0.627450980392157,0.627450980392157);
#16900=COLOUR_RGB('CAD Library Painted - Deep blue',0.0784313725490196,
0.203921568627451,0.349019607843137);
#16901=COLOUR_RGB('CAD Library Painted - Engineering blue',0.12156862745098,
0.356862745098039,0.6);
#16902=COLOUR_RGB('CAD Library Painted - Steel gray',0.592156862745098,
0.631372549019608,0.67843137254902);
#16903=COLOUR_RGB('CAD Library Painted - Graphite',0.168627450980392,0.192156862745098,
0.231372549019608);
#16904=COLOUR_RGB('CAD Library Painted - Light blue',0.286274509803922,
0.552941176470588,0.780392156862745);
#16905=COLOUR_RGB('Dark Blue',0.08,0.2,0.34);
#16906=FILL_AREA_STYLE_COLOUR('',#16905);
#16907=FILL_AREA_STYLE('',(#16906));
#16908=SURFACE_STYLE_FILL_AREA(#16907);
#16909=SURFACE_SIDE_STYLE('',(#16908));
#16910=SURFACE_STYLE_USAGE(.BOTH.,#16909);
#16911=PRESENTATION_STYLE_ASSIGNMENT((#16910));
#16912=COLOUR_RGB('Light Blue',0.38,0.62,0.78);
#16913=FILL_AREA_STYLE_COLOUR('',#16912);
#16914=FILL_AREA_STYLE('',(#16913));
#16915=SURFACE_STYLE_FILL_AREA(#16914);
#16916=SURFACE_SIDE_STYLE('',(#16915));
#16917=SURFACE_STYLE_USAGE(.BOTH.,#16916);
#16918=PRESENTATION_STYLE_ASSIGNMENT((#16917));
#16919=COLOUR_RGB('Sky Blue',0.24,0.69,0.87);
#16920=FILL_AREA_STYLE_COLOUR('',#16919);
#16921=FILL_AREA_STYLE('',(#16920));
#16922=SURFACE_STYLE_FILL_AREA(#16921);
#16923=SURFACE_SIDE_STYLE('',(#16922));
#16924=SURFACE_STYLE_USAGE(.BOTH.,#16923);
#16925=PRESENTATION_STYLE_ASSIGNMENT((#16924));
#16926=COLOUR_RGB('Grey',0.48,0.52,0.57);
#16927=FILL_AREA_STYLE_COLOUR('',#16926);
#16928=FILL_AREA_STYLE('',(#16927));
#16929=SURFACE_STYLE_FILL_AREA(#16928);
#16930=SURFACE_SIDE_STYLE('',(#16929));
#16931=SURFACE_STYLE_USAGE(.BOTH.,#16930);
#16932=PRESENTATION_STYLE_ASSIGNMENT((#16931));
#16933=COLOUR_RGB('Black',0.12,0.14,0.17);
#16934=FILL_AREA_STYLE_COLOUR('',#16933);
#16935=FILL_AREA_STYLE('',(#16934));
#16936=SURFACE_STYLE_FILL_AREA(#16935);
#16937=SURFACE_SIDE_STYLE('',(#16936));
#16938=SURFACE_STYLE_USAGE(.BOTH.,#16937);
#16939=PRESENTATION_STYLE_ASSIGNMENT((#16938));
#16940=COLOUR_RGB('Off White',0.89,0.88,0.83);
#16941=FILL_AREA_STYLE_COLOUR('',#16940);
#16942=FILL_AREA_STYLE('',(#16941));
#16943=SURFACE_STYLE_FILL_AREA(#16942);
#16944=SURFACE_SIDE_STYLE('',(#16943));
#16945=SURFACE_STYLE_USAGE(.BOTH.,#16944);
#16946=PRESENTATION_STYLE_ASSIGNMENT((#16945));
ENDSEC;
END-ISO-10303-21;
